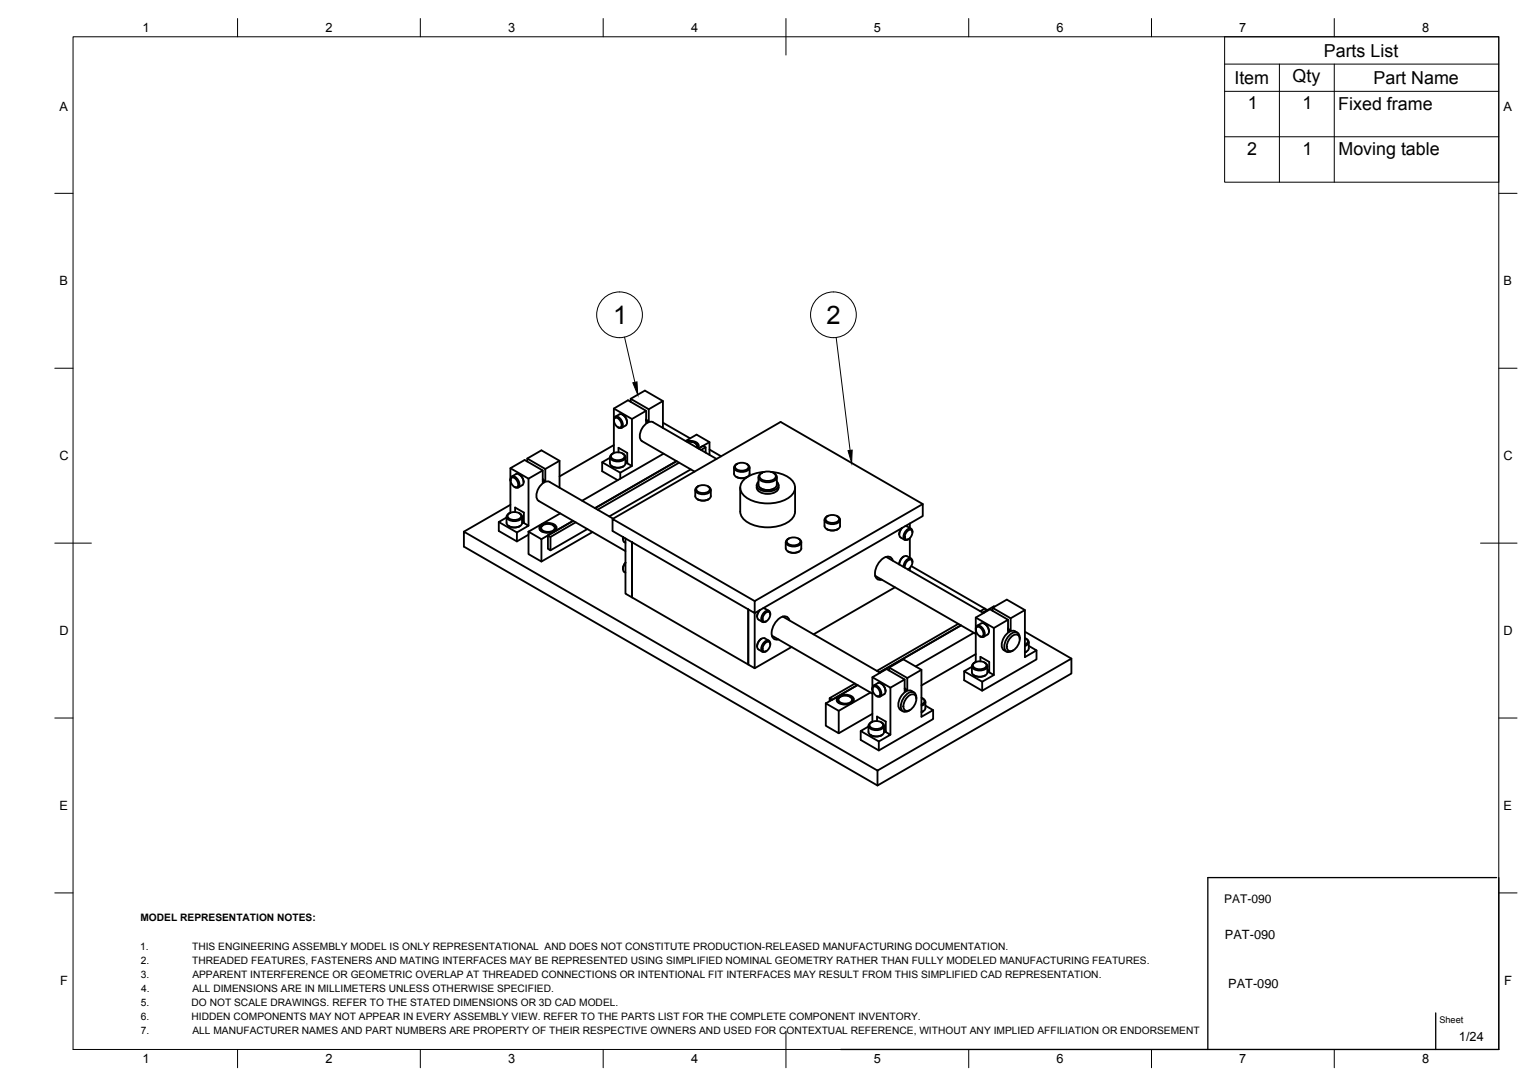
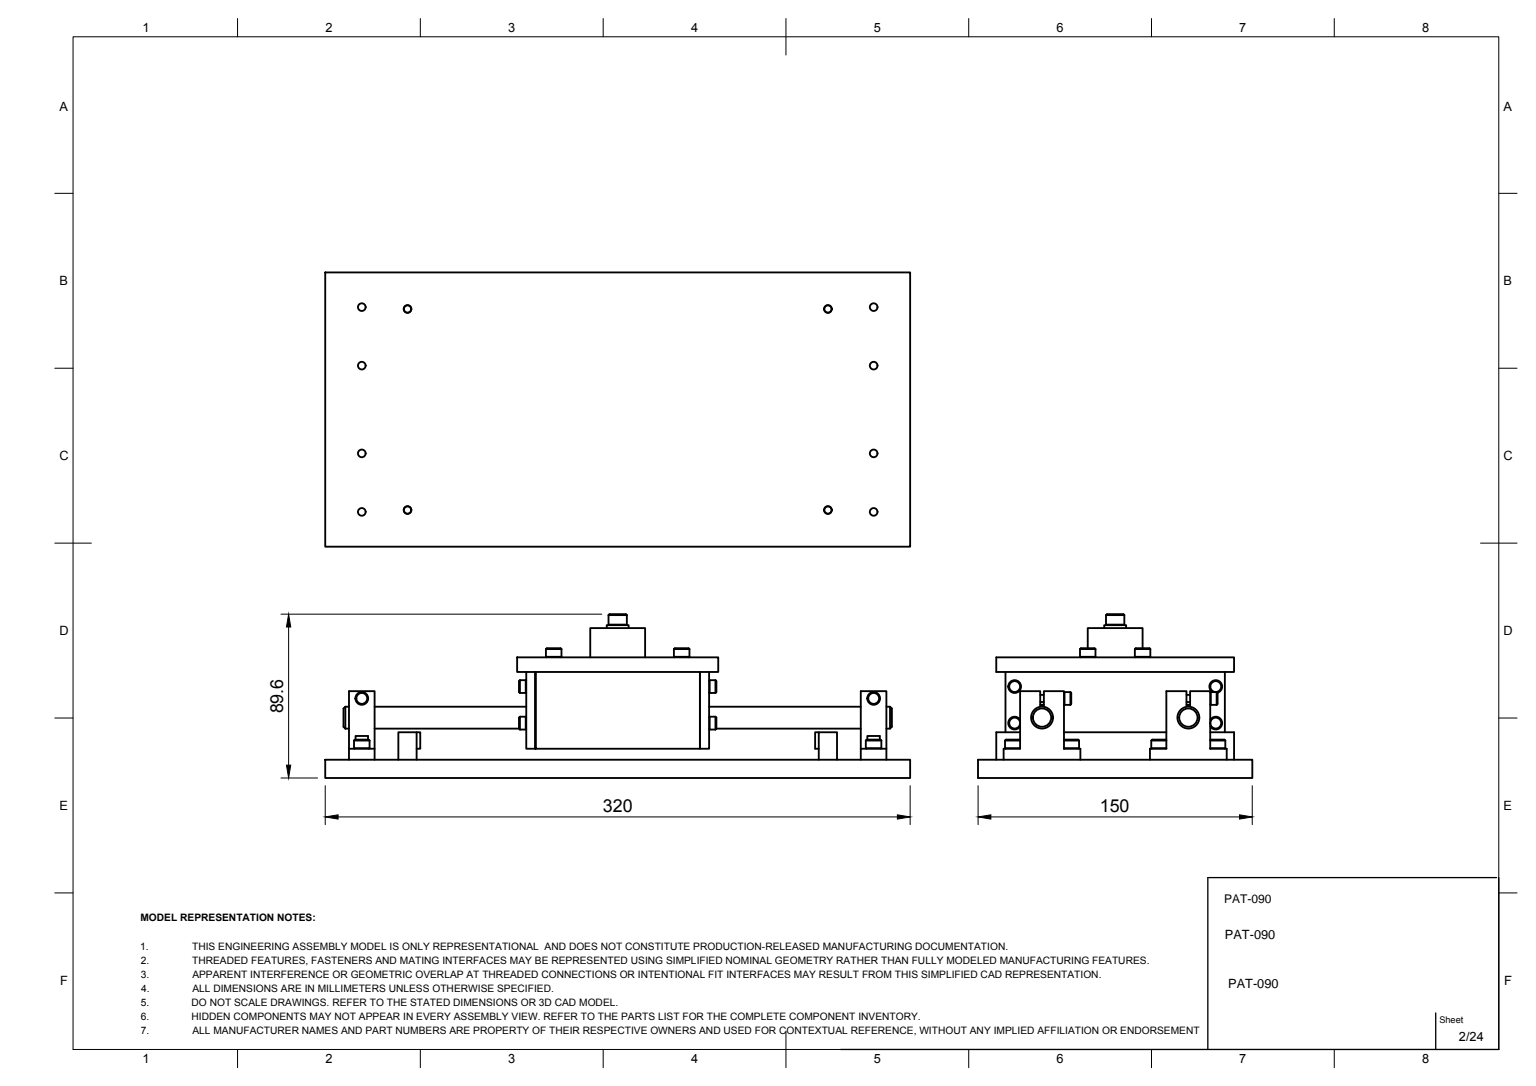
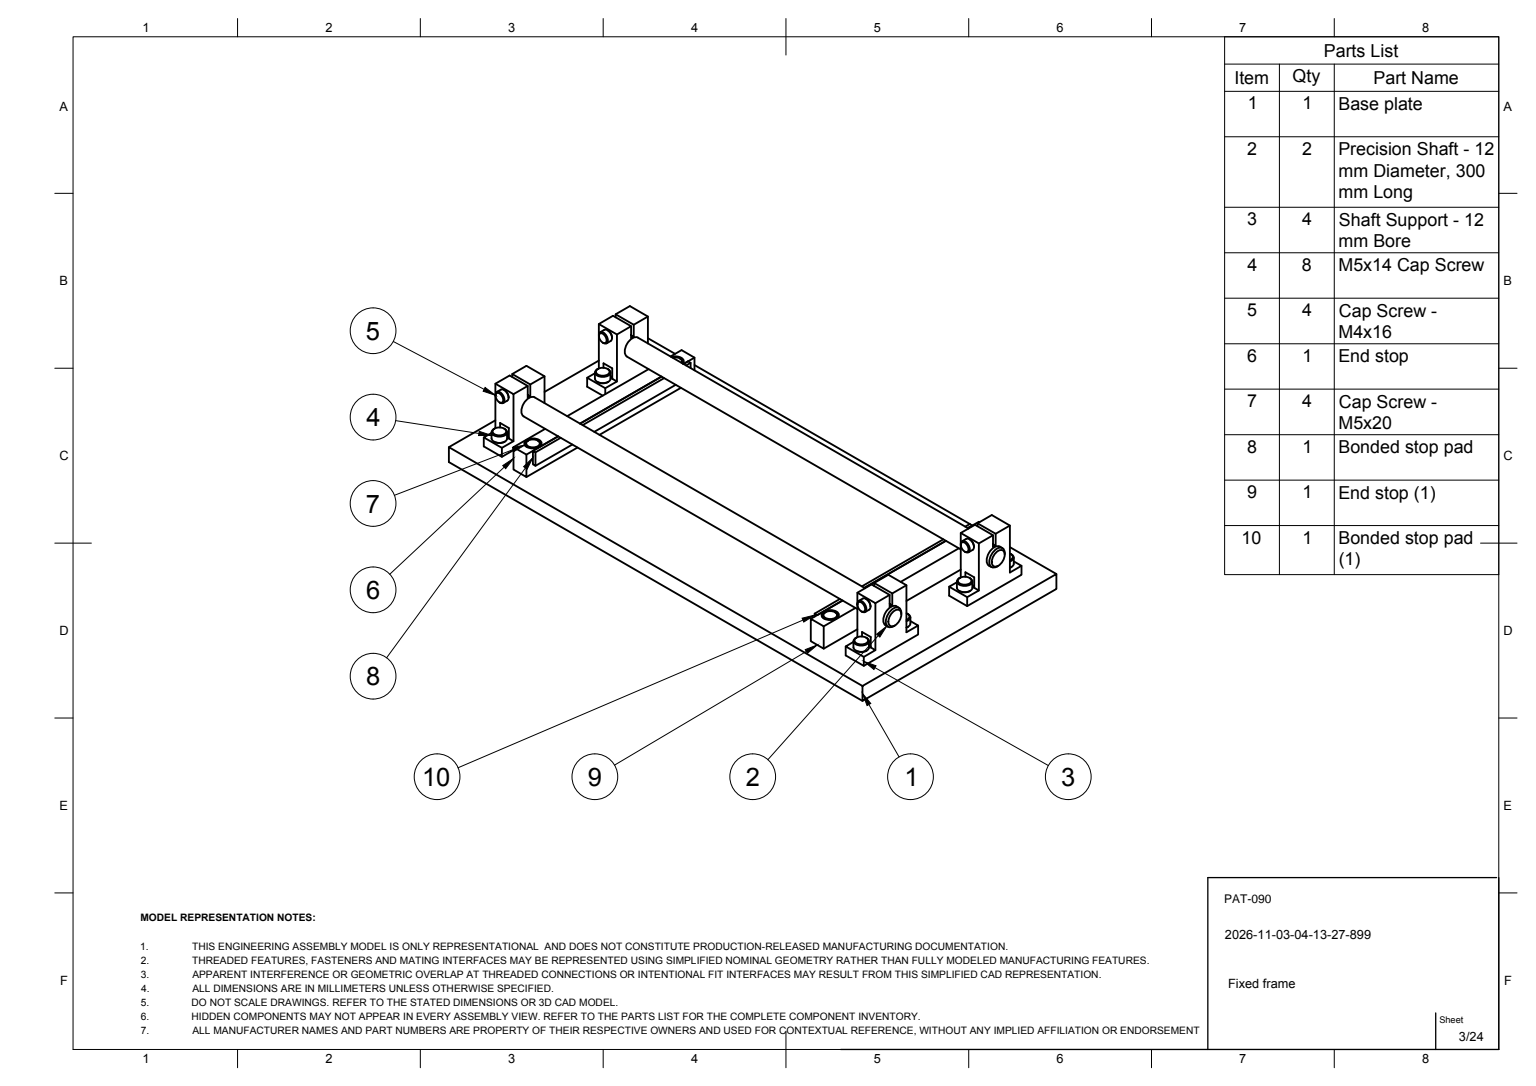
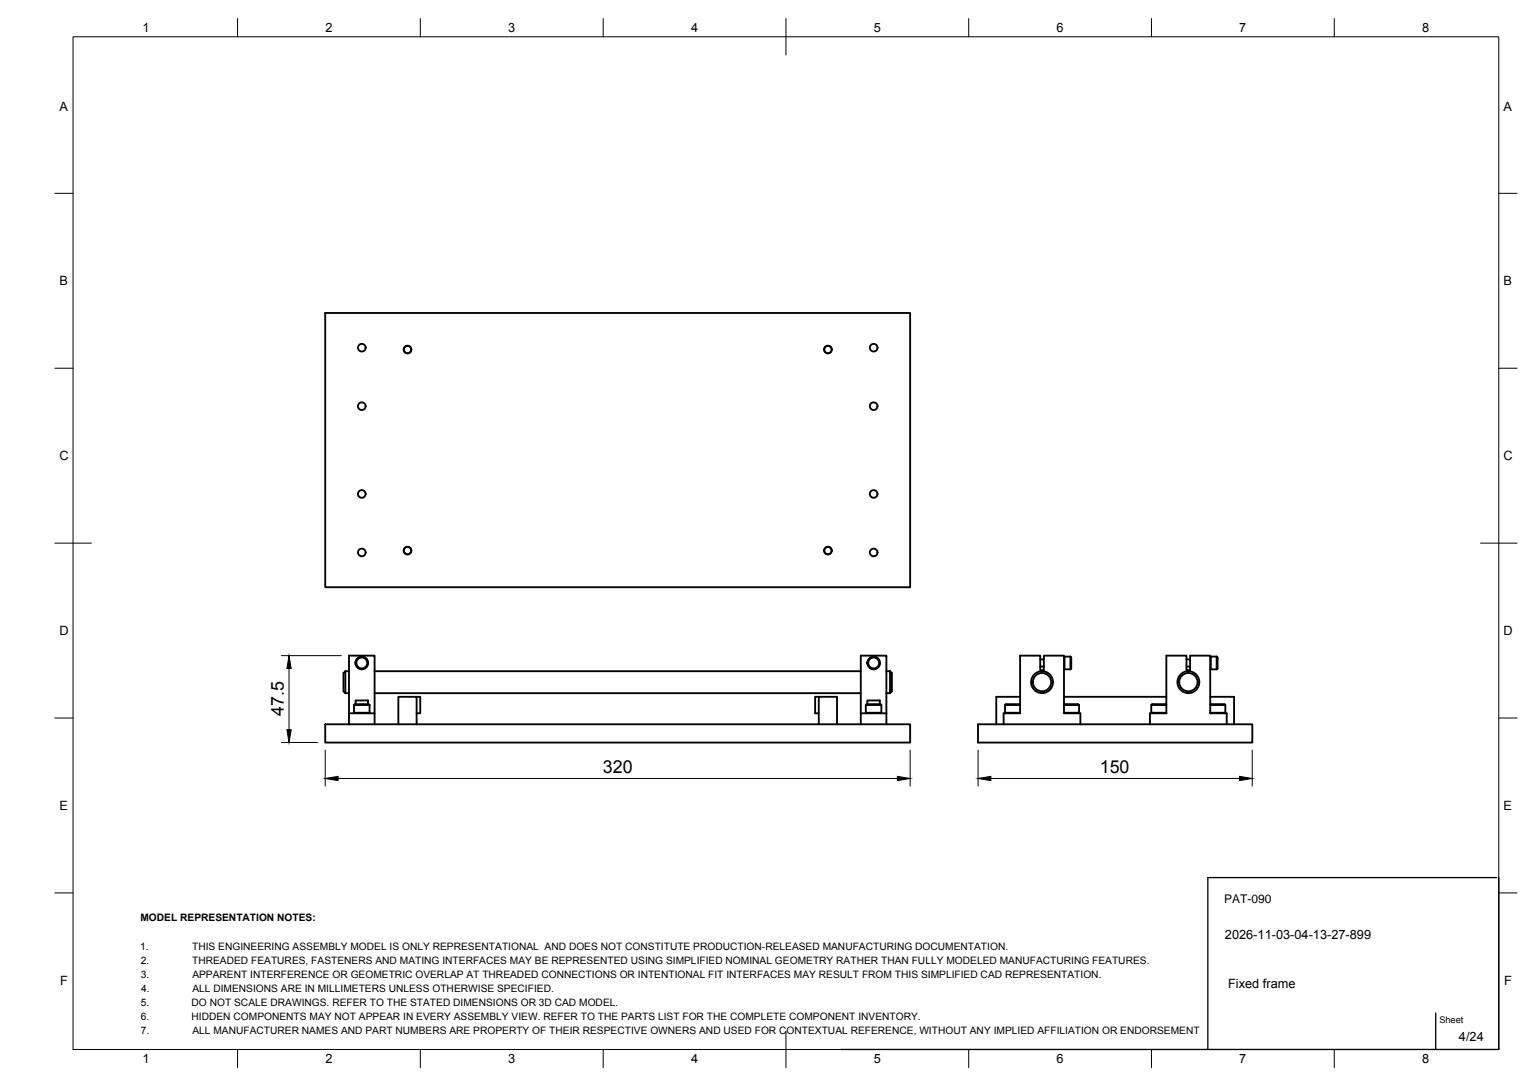
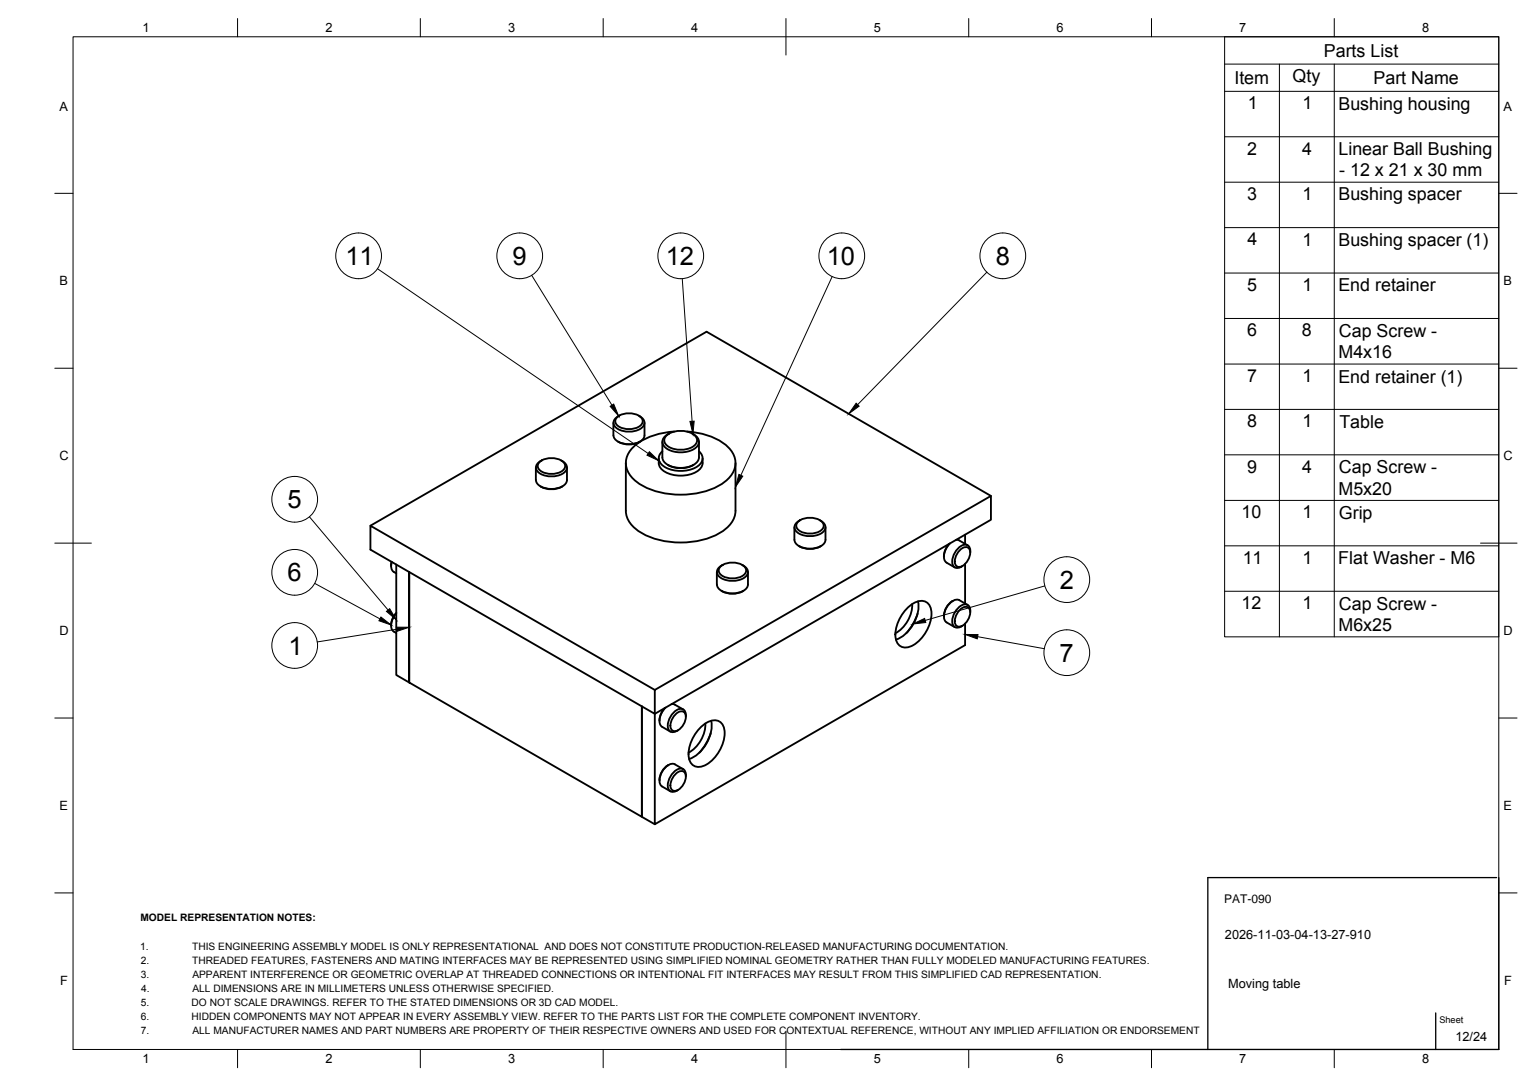
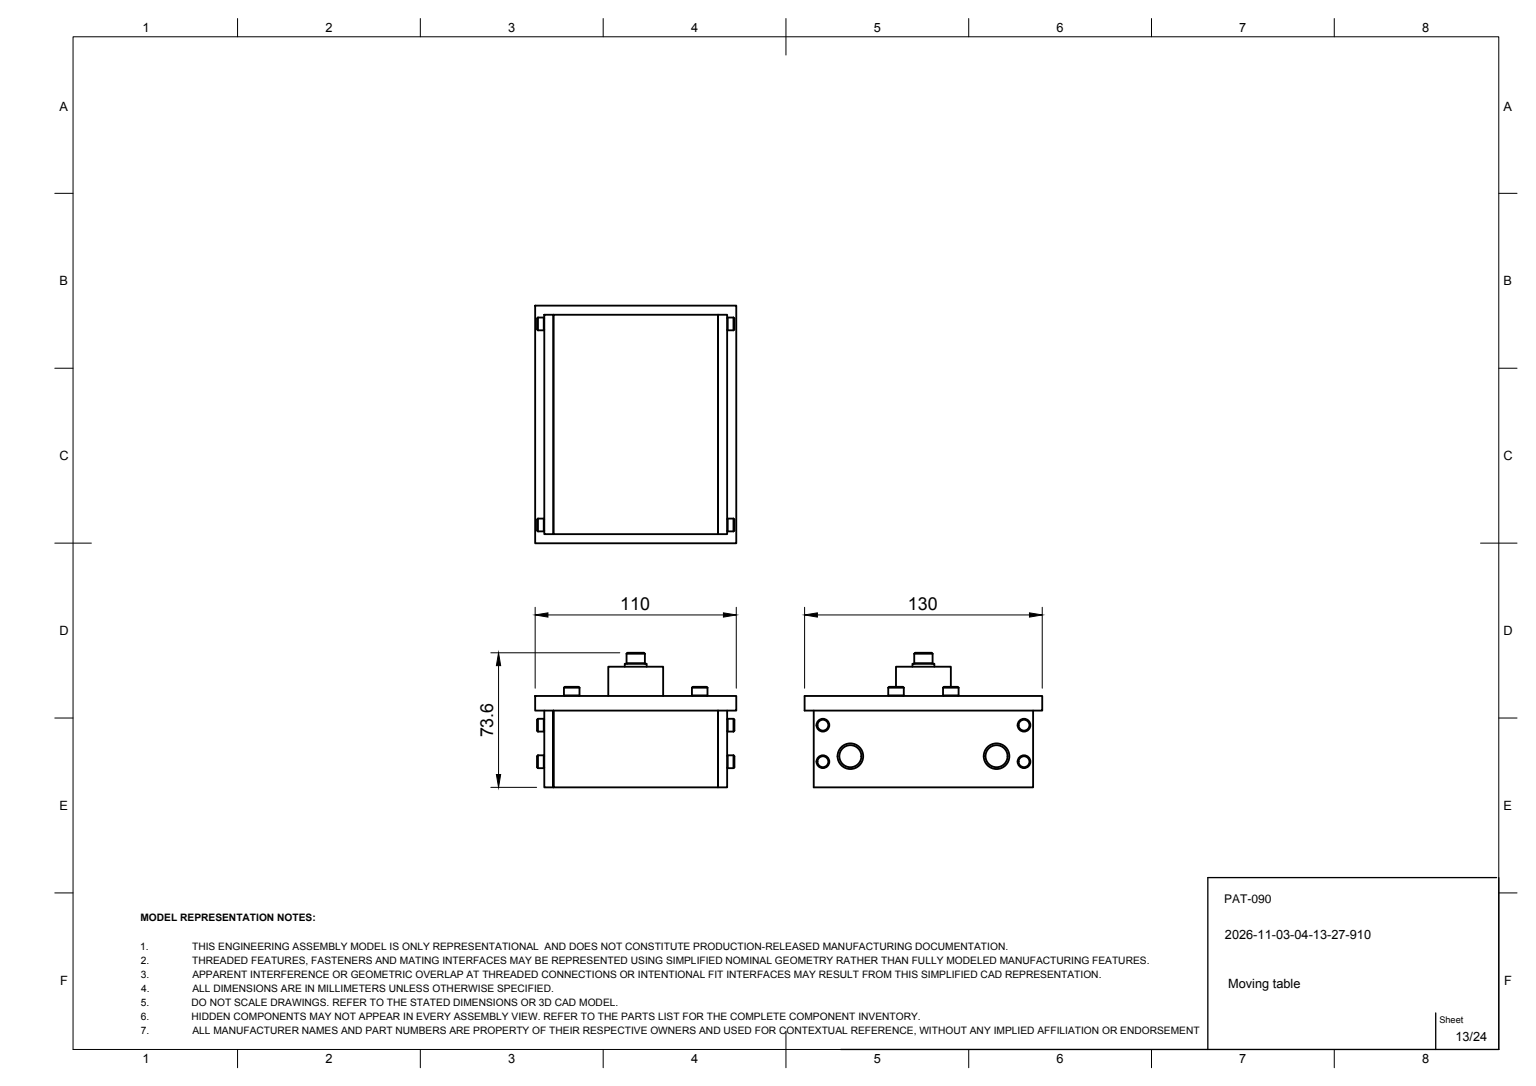
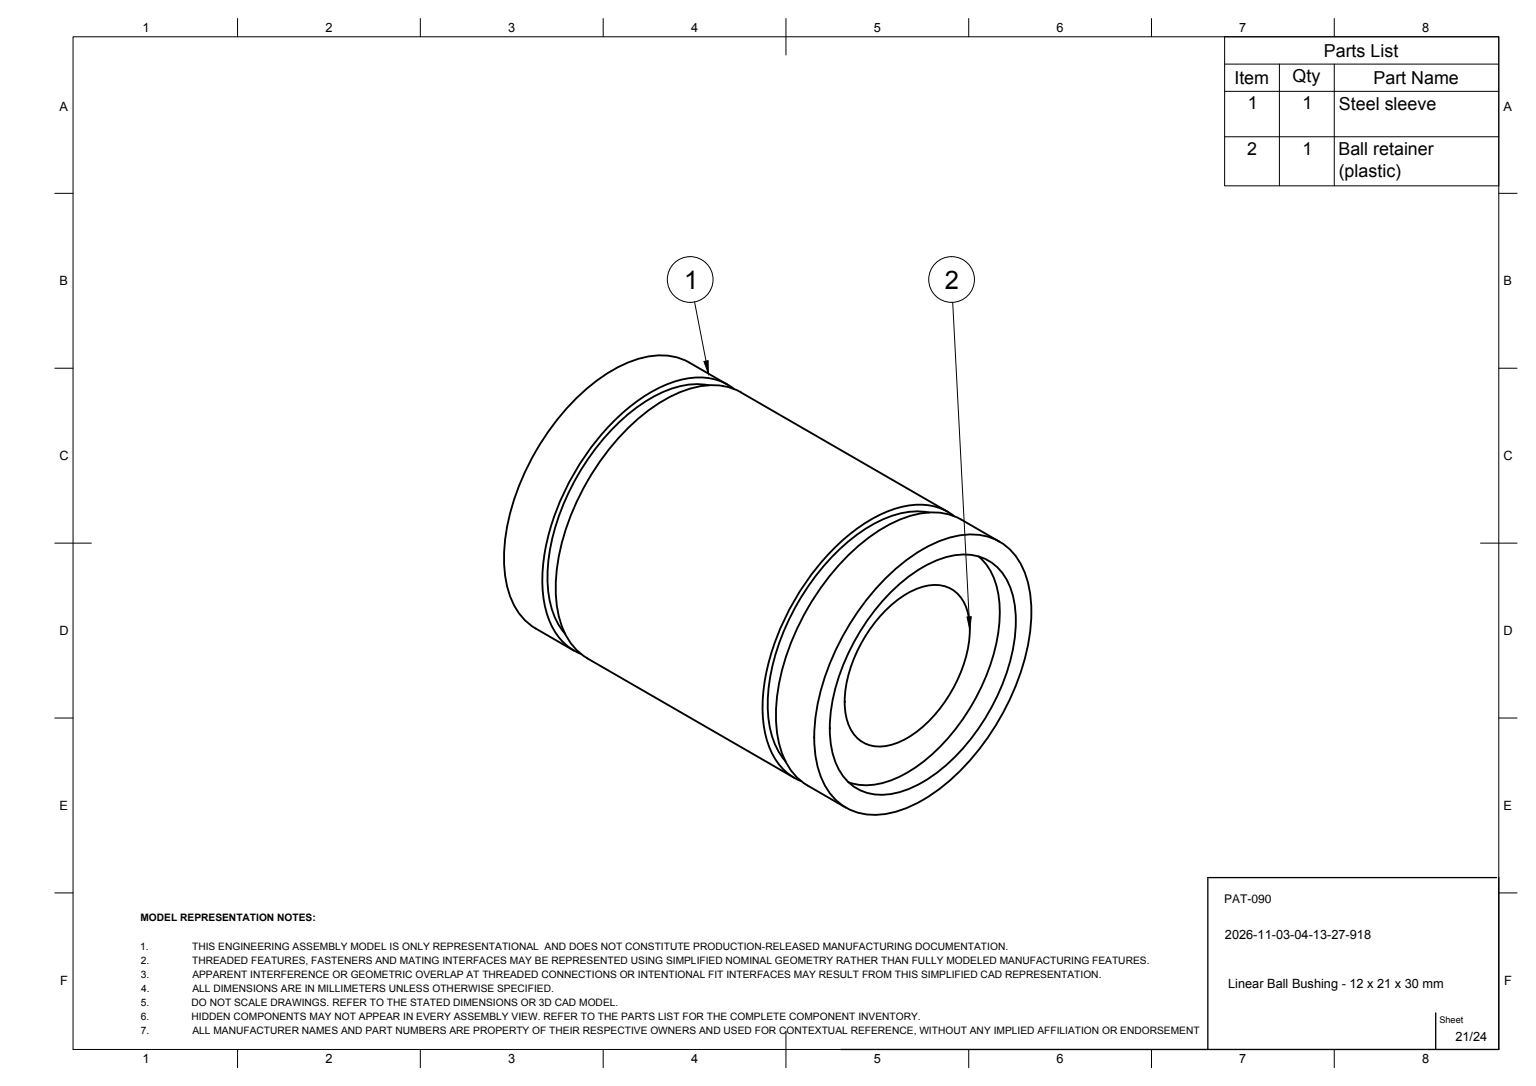
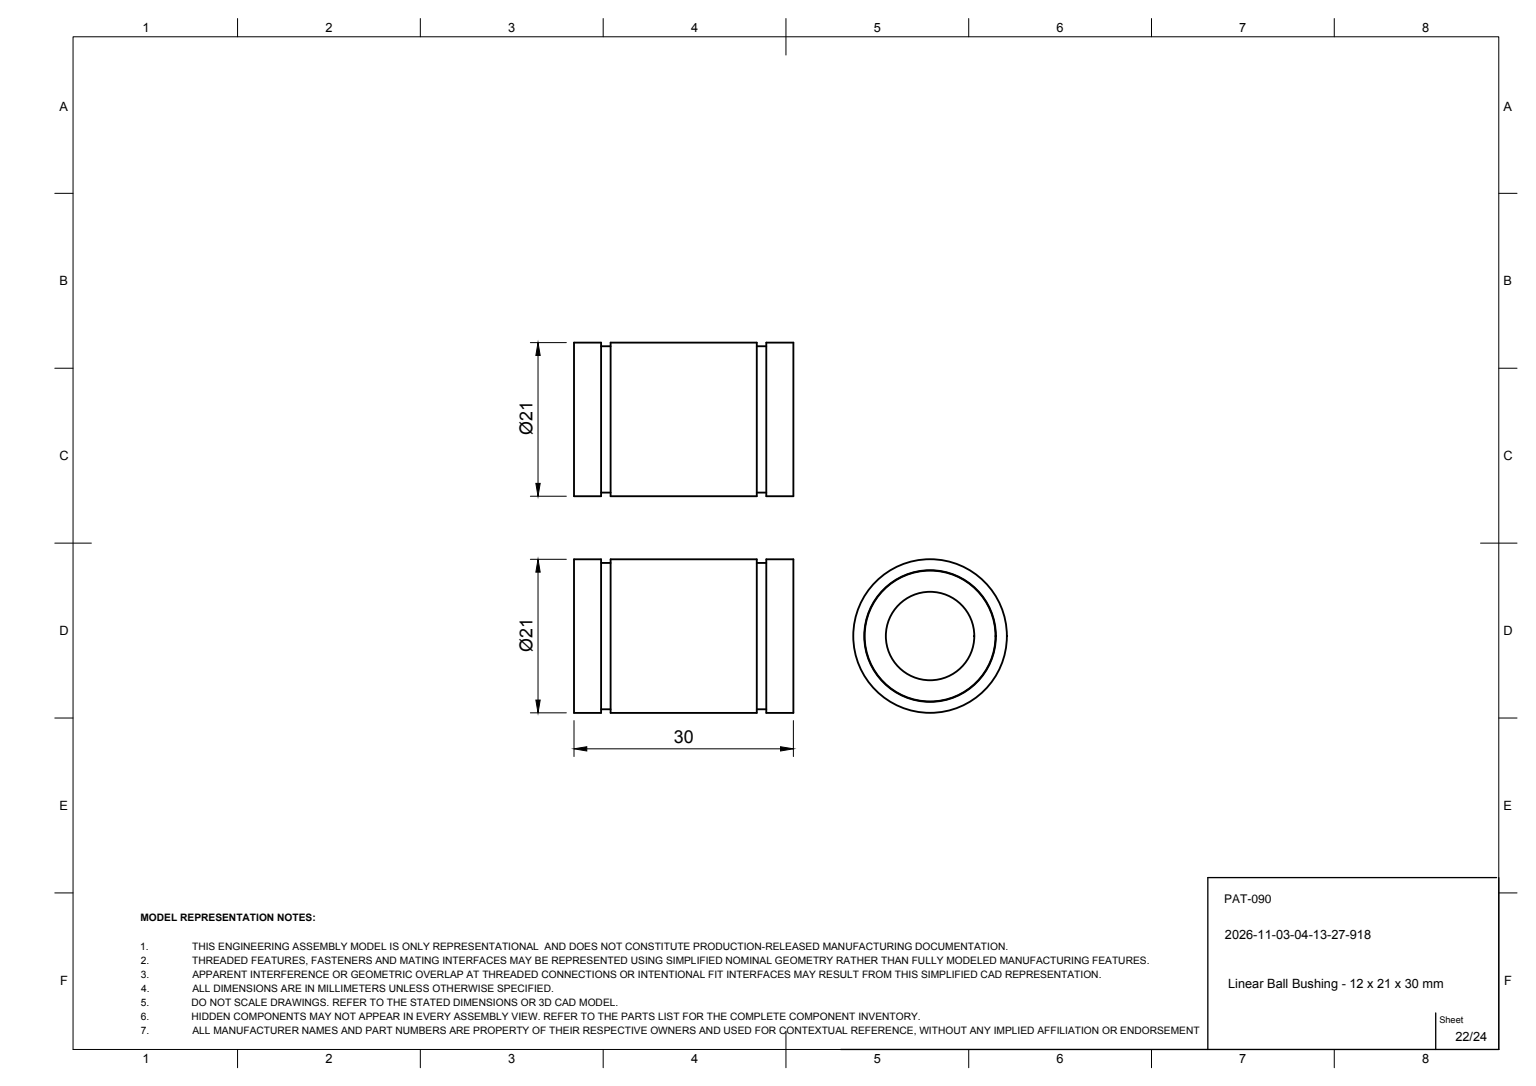
ISO-10303-21;
HEADER;
/* Generated by software containing ST-Developer
 * from STEP Tools, Inc. (www.steptools.com) 
 */

FILE_DESCRIPTION(
/* description */ ('Round-Shaft Linear Stage with Ball Bushings'),
/* implementation_level */ '2;1');

FILE_NAME(
/* name */ 'PAT-090',
/* time_stamp */ '2026-10-27T10:47:55-07:00',
/* author */ (''),
/* organization */ (''),
/* preprocessor_version */ 'ST-DEVELOPER v20.2',
/* originating_system */ 'Autodesk Translation Framework v15.17.0.0',
/* authorisation */ '');

FILE_SCHEMA (('AUTOMOTIVE_DESIGN { 1 0 10303 214 3 1 1 }'));
ENDSEC;

DATA;
#10=MECHANICAL_DESIGN_GEOMETRIC_PRESENTATION_REPRESENTATION('',(#302,#303,
#304,#305,#306,#307,#308,#309,#310,#311,#312,#313,#314,#315,#316,#317,#318,
#319,#320,#321,#322),#7835);
#11=ITEM_DEFINED_TRANSFORMATION($,$,#4984,#5033);
#12=ITEM_DEFINED_TRANSFORMATION($,$,#5016,#5034);
#13=ITEM_DEFINED_TRANSFORMATION($,$,#4651,#5087);
#14=ITEM_DEFINED_TRANSFORMATION($,$,#4694,#5088);
#15=ITEM_DEFINED_TRANSFORMATION($,$,#4715,#5089);
#16=ITEM_DEFINED_TRANSFORMATION($,$,#4722,#5090);
#17=ITEM_DEFINED_TRANSFORMATION($,$,#4743,#5091);
#18=ITEM_DEFINED_TRANSFORMATION($,$,#4750,#5092);
#19=ITEM_DEFINED_TRANSFORMATION($,$,#4760,#5093);
#20=ITEM_DEFINED_TRANSFORMATION($,$,#4798,#5094);
#21=ITEM_DEFINED_TRANSFORMATION($,$,#4798,#5095);
#22=ITEM_DEFINED_TRANSFORMATION($,$,#5035,#5096);
#23=ITEM_DEFINED_TRANSFORMATION($,$,#4760,#5097);
#24=ITEM_DEFINED_TRANSFORMATION($,$,#4798,#5098);
#25=ITEM_DEFINED_TRANSFORMATION($,$,#4798,#5099);
#26=ITEM_DEFINED_TRANSFORMATION($,$,#5035,#5100);
#27=ITEM_DEFINED_TRANSFORMATION($,$,#4750,#5101);
#28=ITEM_DEFINED_TRANSFORMATION($,$,#4760,#5102);
#29=ITEM_DEFINED_TRANSFORMATION($,$,#4798,#5103);
#30=ITEM_DEFINED_TRANSFORMATION($,$,#4798,#5104);
#31=ITEM_DEFINED_TRANSFORMATION($,$,#5035,#5105);
#32=ITEM_DEFINED_TRANSFORMATION($,$,#4760,#5106);
#33=ITEM_DEFINED_TRANSFORMATION($,$,#4798,#5107);
#34=ITEM_DEFINED_TRANSFORMATION($,$,#4798,#5108);
#35=ITEM_DEFINED_TRANSFORMATION($,$,#5035,#5109);
#36=ITEM_DEFINED_TRANSFORMATION($,$,#5061,#5110);
#37=ITEM_DEFINED_TRANSFORMATION($,$,#5061,#5111);
#38=ITEM_DEFINED_TRANSFORMATION($,$,#5061,#5112);
#39=ITEM_DEFINED_TRANSFORMATION($,$,#5061,#5113);
#40=ITEM_DEFINED_TRANSFORMATION($,$,#4823,#5149);
#41=ITEM_DEFINED_TRANSFORMATION($,$,#4884,#5150);
#42=ITEM_DEFINED_TRANSFORMATION($,$,#4893,#5151);
#43=ITEM_DEFINED_TRANSFORMATION($,$,#4902,#5152);
#44=ITEM_DEFINED_TRANSFORMATION($,$,#4927,#5153);
#45=ITEM_DEFINED_TRANSFORMATION($,$,#4952,#5154);
#46=ITEM_DEFINED_TRANSFORMATION($,$,#4974,#5155);
#47=ITEM_DEFINED_TRANSFORMATION($,$,#4983,#5156);
#48=ITEM_DEFINED_TRANSFORMATION($,$,#4983,#5157);
#49=ITEM_DEFINED_TRANSFORMATION($,$,#4983,#5158);
#50=ITEM_DEFINED_TRANSFORMATION($,$,#4983,#5159);
#51=ITEM_DEFINED_TRANSFORMATION($,$,#5035,#5160);
#52=ITEM_DEFINED_TRANSFORMATION($,$,#5035,#5161);
#53=ITEM_DEFINED_TRANSFORMATION($,$,#5035,#5162);
#54=ITEM_DEFINED_TRANSFORMATION($,$,#5035,#5163);
#55=ITEM_DEFINED_TRANSFORMATION($,$,#5035,#5164);
#56=ITEM_DEFINED_TRANSFORMATION($,$,#5035,#5165);
#57=ITEM_DEFINED_TRANSFORMATION($,$,#5035,#5166);
#58=ITEM_DEFINED_TRANSFORMATION($,$,#5035,#5167);
#59=ITEM_DEFINED_TRANSFORMATION($,$,#5061,#5168);
#60=ITEM_DEFINED_TRANSFORMATION($,$,#5061,#5169);
#61=ITEM_DEFINED_TRANSFORMATION($,$,#5061,#5170);
#62=ITEM_DEFINED_TRANSFORMATION($,$,#5061,#5171);
#63=ITEM_DEFINED_TRANSFORMATION($,$,#5114,#5172);
#64=ITEM_DEFINED_TRANSFORMATION($,$,#5123,#5173);
#65=ITEM_DEFINED_TRANSFORMATION($,$,#4650,#5174);
#66=ITEM_DEFINED_TRANSFORMATION($,$,#4822,#5175);
#67=(
REPRESENTATION_RELATIONSHIP($,$,#7965,#7964)
REPRESENTATION_RELATIONSHIP_WITH_TRANSFORMATION(#11)
SHAPE_REPRESENTATION_RELATIONSHIP()
);
#68=(
REPRESENTATION_RELATIONSHIP($,$,#7966,#7964)
REPRESENTATION_RELATIONSHIP_WITH_TRANSFORMATION(#12)
SHAPE_REPRESENTATION_RELATIONSHIP()
);
#69=(
REPRESENTATION_RELATIONSHIP($,$,#7948,#7947)
REPRESENTATION_RELATIONSHIP_WITH_TRANSFORMATION(#13)
SHAPE_REPRESENTATION_RELATIONSHIP()
);
#70=(
REPRESENTATION_RELATIONSHIP($,$,#7949,#7947)
REPRESENTATION_RELATIONSHIP_WITH_TRANSFORMATION(#14)
SHAPE_REPRESENTATION_RELATIONSHIP()
);
#71=(
REPRESENTATION_RELATIONSHIP($,$,#7950,#7947)
REPRESENTATION_RELATIONSHIP_WITH_TRANSFORMATION(#15)
SHAPE_REPRESENTATION_RELATIONSHIP()
);
#72=(
REPRESENTATION_RELATIONSHIP($,$,#7951,#7947)
REPRESENTATION_RELATIONSHIP_WITH_TRANSFORMATION(#16)
SHAPE_REPRESENTATION_RELATIONSHIP()
);
#73=(
REPRESENTATION_RELATIONSHIP($,$,#7952,#7947)
REPRESENTATION_RELATIONSHIP_WITH_TRANSFORMATION(#17)
SHAPE_REPRESENTATION_RELATIONSHIP()
);
#74=(
REPRESENTATION_RELATIONSHIP($,$,#7953,#7947)
REPRESENTATION_RELATIONSHIP_WITH_TRANSFORMATION(#18)
SHAPE_REPRESENTATION_RELATIONSHIP()
);
#75=(
REPRESENTATION_RELATIONSHIP($,$,#7954,#7947)
REPRESENTATION_RELATIONSHIP_WITH_TRANSFORMATION(#19)
SHAPE_REPRESENTATION_RELATIONSHIP()
);
#76=(
REPRESENTATION_RELATIONSHIP($,$,#7955,#7947)
REPRESENTATION_RELATIONSHIP_WITH_TRANSFORMATION(#20)
SHAPE_REPRESENTATION_RELATIONSHIP()
);
#77=(
REPRESENTATION_RELATIONSHIP($,$,#7955,#7947)
REPRESENTATION_RELATIONSHIP_WITH_TRANSFORMATION(#21)
SHAPE_REPRESENTATION_RELATIONSHIP()
);
#78=(
REPRESENTATION_RELATIONSHIP($,$,#7967,#7947)
REPRESENTATION_RELATIONSHIP_WITH_TRANSFORMATION(#22)
SHAPE_REPRESENTATION_RELATIONSHIP()
);
#79=(
REPRESENTATION_RELATIONSHIP($,$,#7954,#7947)
REPRESENTATION_RELATIONSHIP_WITH_TRANSFORMATION(#23)
SHAPE_REPRESENTATION_RELATIONSHIP()
);
#80=(
REPRESENTATION_RELATIONSHIP($,$,#7955,#7947)
REPRESENTATION_RELATIONSHIP_WITH_TRANSFORMATION(#24)
SHAPE_REPRESENTATION_RELATIONSHIP()
);
#81=(
REPRESENTATION_RELATIONSHIP($,$,#7955,#7947)
REPRESENTATION_RELATIONSHIP_WITH_TRANSFORMATION(#25)
SHAPE_REPRESENTATION_RELATIONSHIP()
);
#82=(
REPRESENTATION_RELATIONSHIP($,$,#7967,#7947)
REPRESENTATION_RELATIONSHIP_WITH_TRANSFORMATION(#26)
SHAPE_REPRESENTATION_RELATIONSHIP()
);
#83=(
REPRESENTATION_RELATIONSHIP($,$,#7953,#7947)
REPRESENTATION_RELATIONSHIP_WITH_TRANSFORMATION(#27)
SHAPE_REPRESENTATION_RELATIONSHIP()
);
#84=(
REPRESENTATION_RELATIONSHIP($,$,#7954,#7947)
REPRESENTATION_RELATIONSHIP_WITH_TRANSFORMATION(#28)
SHAPE_REPRESENTATION_RELATIONSHIP()
);
#85=(
REPRESENTATION_RELATIONSHIP($,$,#7955,#7947)
REPRESENTATION_RELATIONSHIP_WITH_TRANSFORMATION(#29)
SHAPE_REPRESENTATION_RELATIONSHIP()
);
#86=(
REPRESENTATION_RELATIONSHIP($,$,#7955,#7947)
REPRESENTATION_RELATIONSHIP_WITH_TRANSFORMATION(#30)
SHAPE_REPRESENTATION_RELATIONSHIP()
);
#87=(
REPRESENTATION_RELATIONSHIP($,$,#7967,#7947)
REPRESENTATION_RELATIONSHIP_WITH_TRANSFORMATION(#31)
SHAPE_REPRESENTATION_RELATIONSHIP()
);
#88=(
REPRESENTATION_RELATIONSHIP($,$,#7954,#7947)
REPRESENTATION_RELATIONSHIP_WITH_TRANSFORMATION(#32)
SHAPE_REPRESENTATION_RELATIONSHIP()
);
#89=(
REPRESENTATION_RELATIONSHIP($,$,#7955,#7947)
REPRESENTATION_RELATIONSHIP_WITH_TRANSFORMATION(#33)
SHAPE_REPRESENTATION_RELATIONSHIP()
);
#90=(
REPRESENTATION_RELATIONSHIP($,$,#7955,#7947)
REPRESENTATION_RELATIONSHIP_WITH_TRANSFORMATION(#34)
SHAPE_REPRESENTATION_RELATIONSHIP()
);
#91=(
REPRESENTATION_RELATIONSHIP($,$,#7967,#7947)
REPRESENTATION_RELATIONSHIP_WITH_TRANSFORMATION(#35)
SHAPE_REPRESENTATION_RELATIONSHIP()
);
#92=(
REPRESENTATION_RELATIONSHIP($,$,#7968,#7947)
REPRESENTATION_RELATIONSHIP_WITH_TRANSFORMATION(#36)
SHAPE_REPRESENTATION_RELATIONSHIP()
);
#93=(
REPRESENTATION_RELATIONSHIP($,$,#7968,#7947)
REPRESENTATION_RELATIONSHIP_WITH_TRANSFORMATION(#37)
SHAPE_REPRESENTATION_RELATIONSHIP()
);
#94=(
REPRESENTATION_RELATIONSHIP($,$,#7968,#7947)
REPRESENTATION_RELATIONSHIP_WITH_TRANSFORMATION(#38)
SHAPE_REPRESENTATION_RELATIONSHIP()
);
#95=(
REPRESENTATION_RELATIONSHIP($,$,#7968,#7947)
REPRESENTATION_RELATIONSHIP_WITH_TRANSFORMATION(#39)
SHAPE_REPRESENTATION_RELATIONSHIP()
);
#96=(
REPRESENTATION_RELATIONSHIP($,$,#7957,#7956)
REPRESENTATION_RELATIONSHIP_WITH_TRANSFORMATION(#40)
SHAPE_REPRESENTATION_RELATIONSHIP()
);
#97=(
REPRESENTATION_RELATIONSHIP($,$,#7958,#7956)
REPRESENTATION_RELATIONSHIP_WITH_TRANSFORMATION(#41)
SHAPE_REPRESENTATION_RELATIONSHIP()
);
#98=(
REPRESENTATION_RELATIONSHIP($,$,#7959,#7956)
REPRESENTATION_RELATIONSHIP_WITH_TRANSFORMATION(#42)
SHAPE_REPRESENTATION_RELATIONSHIP()
);
#99=(
REPRESENTATION_RELATIONSHIP($,$,#7960,#7956)
REPRESENTATION_RELATIONSHIP_WITH_TRANSFORMATION(#43)
SHAPE_REPRESENTATION_RELATIONSHIP()
);
#100=(
REPRESENTATION_RELATIONSHIP($,$,#7961,#7956)
REPRESENTATION_RELATIONSHIP_WITH_TRANSFORMATION(#44)
SHAPE_REPRESENTATION_RELATIONSHIP()
);
#101=(
REPRESENTATION_RELATIONSHIP($,$,#7962,#7956)
REPRESENTATION_RELATIONSHIP_WITH_TRANSFORMATION(#45)
SHAPE_REPRESENTATION_RELATIONSHIP()
);
#102=(
REPRESENTATION_RELATIONSHIP($,$,#7963,#7956)
REPRESENTATION_RELATIONSHIP_WITH_TRANSFORMATION(#46)
SHAPE_REPRESENTATION_RELATIONSHIP()
);
#103=(
REPRESENTATION_RELATIONSHIP($,$,#7964,#7956)
REPRESENTATION_RELATIONSHIP_WITH_TRANSFORMATION(#47)
SHAPE_REPRESENTATION_RELATIONSHIP()
);
#104=(
REPRESENTATION_RELATIONSHIP($,$,#7964,#7956)
REPRESENTATION_RELATIONSHIP_WITH_TRANSFORMATION(#48)
SHAPE_REPRESENTATION_RELATIONSHIP()
);
#105=(
REPRESENTATION_RELATIONSHIP($,$,#7964,#7956)
REPRESENTATION_RELATIONSHIP_WITH_TRANSFORMATION(#49)
SHAPE_REPRESENTATION_RELATIONSHIP()
);
#106=(
REPRESENTATION_RELATIONSHIP($,$,#7964,#7956)
REPRESENTATION_RELATIONSHIP_WITH_TRANSFORMATION(#50)
SHAPE_REPRESENTATION_RELATIONSHIP()
);
#107=(
REPRESENTATION_RELATIONSHIP($,$,#7967,#7956)
REPRESENTATION_RELATIONSHIP_WITH_TRANSFORMATION(#51)
SHAPE_REPRESENTATION_RELATIONSHIP()
);
#108=(
REPRESENTATION_RELATIONSHIP($,$,#7967,#7956)
REPRESENTATION_RELATIONSHIP_WITH_TRANSFORMATION(#52)
SHAPE_REPRESENTATION_RELATIONSHIP()
);
#109=(
REPRESENTATION_RELATIONSHIP($,$,#7967,#7956)
REPRESENTATION_RELATIONSHIP_WITH_TRANSFORMATION(#53)
SHAPE_REPRESENTATION_RELATIONSHIP()
);
#110=(
REPRESENTATION_RELATIONSHIP($,$,#7967,#7956)
REPRESENTATION_RELATIONSHIP_WITH_TRANSFORMATION(#54)
SHAPE_REPRESENTATION_RELATIONSHIP()
);
#111=(
REPRESENTATION_RELATIONSHIP($,$,#7967,#7956)
REPRESENTATION_RELATIONSHIP_WITH_TRANSFORMATION(#55)
SHAPE_REPRESENTATION_RELATIONSHIP()
);
#112=(
REPRESENTATION_RELATIONSHIP($,$,#7967,#7956)
REPRESENTATION_RELATIONSHIP_WITH_TRANSFORMATION(#56)
SHAPE_REPRESENTATION_RELATIONSHIP()
);
#113=(
REPRESENTATION_RELATIONSHIP($,$,#7967,#7956)
REPRESENTATION_RELATIONSHIP_WITH_TRANSFORMATION(#57)
SHAPE_REPRESENTATION_RELATIONSHIP()
);
#114=(
REPRESENTATION_RELATIONSHIP($,$,#7967,#7956)
REPRESENTATION_RELATIONSHIP_WITH_TRANSFORMATION(#58)
SHAPE_REPRESENTATION_RELATIONSHIP()
);
#115=(
REPRESENTATION_RELATIONSHIP($,$,#7968,#7956)
REPRESENTATION_RELATIONSHIP_WITH_TRANSFORMATION(#59)
SHAPE_REPRESENTATION_RELATIONSHIP()
);
#116=(
REPRESENTATION_RELATIONSHIP($,$,#7968,#7956)
REPRESENTATION_RELATIONSHIP_WITH_TRANSFORMATION(#60)
SHAPE_REPRESENTATION_RELATIONSHIP()
);
#117=(
REPRESENTATION_RELATIONSHIP($,$,#7968,#7956)
REPRESENTATION_RELATIONSHIP_WITH_TRANSFORMATION(#61)
SHAPE_REPRESENTATION_RELATIONSHIP()
);
#118=(
REPRESENTATION_RELATIONSHIP($,$,#7968,#7956)
REPRESENTATION_RELATIONSHIP_WITH_TRANSFORMATION(#62)
SHAPE_REPRESENTATION_RELATIONSHIP()
);
#119=(
REPRESENTATION_RELATIONSHIP($,$,#7969,#7956)
REPRESENTATION_RELATIONSHIP_WITH_TRANSFORMATION(#63)
SHAPE_REPRESENTATION_RELATIONSHIP()
);
#120=(
REPRESENTATION_RELATIONSHIP($,$,#7970,#7956)
REPRESENTATION_RELATIONSHIP_WITH_TRANSFORMATION(#64)
SHAPE_REPRESENTATION_RELATIONSHIP()
);
#121=(
REPRESENTATION_RELATIONSHIP($,$,#7947,#7946)
REPRESENTATION_RELATIONSHIP_WITH_TRANSFORMATION(#65)
SHAPE_REPRESENTATION_RELATIONSHIP()
);
#122=(
REPRESENTATION_RELATIONSHIP($,$,#7956,#7946)
REPRESENTATION_RELATIONSHIP_WITH_TRANSFORMATION(#66)
SHAPE_REPRESENTATION_RELATIONSHIP()
);
#123=CONTEXT_DEPENDENT_SHAPE_REPRESENTATION(#67,#7886);
#124=CONTEXT_DEPENDENT_SHAPE_REPRESENTATION(#68,#7887);
#125=CONTEXT_DEPENDENT_SHAPE_REPRESENTATION(#69,#7890);
#126=CONTEXT_DEPENDENT_SHAPE_REPRESENTATION(#70,#7891);
#127=CONTEXT_DEPENDENT_SHAPE_REPRESENTATION(#71,#7892);
#128=CONTEXT_DEPENDENT_SHAPE_REPRESENTATION(#72,#7893);
#129=CONTEXT_DEPENDENT_SHAPE_REPRESENTATION(#73,#7894);
#130=CONTEXT_DEPENDENT_SHAPE_REPRESENTATION(#74,#7895);
#131=CONTEXT_DEPENDENT_SHAPE_REPRESENTATION(#75,#7896);
#132=CONTEXT_DEPENDENT_SHAPE_REPRESENTATION(#76,#7897);
#133=CONTEXT_DEPENDENT_SHAPE_REPRESENTATION(#77,#7898);
#134=CONTEXT_DEPENDENT_SHAPE_REPRESENTATION(#78,#7899);
#135=CONTEXT_DEPENDENT_SHAPE_REPRESENTATION(#79,#7900);
#136=CONTEXT_DEPENDENT_SHAPE_REPRESENTATION(#80,#7901);
#137=CONTEXT_DEPENDENT_SHAPE_REPRESENTATION(#81,#7902);
#138=CONTEXT_DEPENDENT_SHAPE_REPRESENTATION(#82,#7903);
#139=CONTEXT_DEPENDENT_SHAPE_REPRESENTATION(#83,#7904);
#140=CONTEXT_DEPENDENT_SHAPE_REPRESENTATION(#84,#7905);
#141=CONTEXT_DEPENDENT_SHAPE_REPRESENTATION(#85,#7906);
#142=CONTEXT_DEPENDENT_SHAPE_REPRESENTATION(#86,#7907);
#143=CONTEXT_DEPENDENT_SHAPE_REPRESENTATION(#87,#7908);
#144=CONTEXT_DEPENDENT_SHAPE_REPRESENTATION(#88,#7909);
#145=CONTEXT_DEPENDENT_SHAPE_REPRESENTATION(#89,#7910);
#146=CONTEXT_DEPENDENT_SHAPE_REPRESENTATION(#90,#7911);
#147=CONTEXT_DEPENDENT_SHAPE_REPRESENTATION(#91,#7912);
#148=CONTEXT_DEPENDENT_SHAPE_REPRESENTATION(#92,#7913);
#149=CONTEXT_DEPENDENT_SHAPE_REPRESENTATION(#93,#7914);
#150=CONTEXT_DEPENDENT_SHAPE_REPRESENTATION(#94,#7915);
#151=CONTEXT_DEPENDENT_SHAPE_REPRESENTATION(#95,#7916);
#152=CONTEXT_DEPENDENT_SHAPE_REPRESENTATION(#96,#7919);
#153=CONTEXT_DEPENDENT_SHAPE_REPRESENTATION(#97,#7920);
#154=CONTEXT_DEPENDENT_SHAPE_REPRESENTATION(#98,#7921);
#155=CONTEXT_DEPENDENT_SHAPE_REPRESENTATION(#99,#7922);
#156=CONTEXT_DEPENDENT_SHAPE_REPRESENTATION(#100,#7923);
#157=CONTEXT_DEPENDENT_SHAPE_REPRESENTATION(#101,#7924);
#158=CONTEXT_DEPENDENT_SHAPE_REPRESENTATION(#102,#7925);
#159=CONTEXT_DEPENDENT_SHAPE_REPRESENTATION(#103,#7926);
#160=CONTEXT_DEPENDENT_SHAPE_REPRESENTATION(#104,#7927);
#161=CONTEXT_DEPENDENT_SHAPE_REPRESENTATION(#105,#7928);
#162=CONTEXT_DEPENDENT_SHAPE_REPRESENTATION(#106,#7929);
#163=CONTEXT_DEPENDENT_SHAPE_REPRESENTATION(#107,#7930);
#164=CONTEXT_DEPENDENT_SHAPE_REPRESENTATION(#108,#7931);
#165=CONTEXT_DEPENDENT_SHAPE_REPRESENTATION(#109,#7932);
#166=CONTEXT_DEPENDENT_SHAPE_REPRESENTATION(#110,#7933);
#167=CONTEXT_DEPENDENT_SHAPE_REPRESENTATION(#111,#7934);
#168=CONTEXT_DEPENDENT_SHAPE_REPRESENTATION(#112,#7935);
#169=CONTEXT_DEPENDENT_SHAPE_REPRESENTATION(#113,#7936);
#170=CONTEXT_DEPENDENT_SHAPE_REPRESENTATION(#114,#7937);
#171=CONTEXT_DEPENDENT_SHAPE_REPRESENTATION(#115,#7938);
#172=CONTEXT_DEPENDENT_SHAPE_REPRESENTATION(#116,#7939);
#173=CONTEXT_DEPENDENT_SHAPE_REPRESENTATION(#117,#7940);
#174=CONTEXT_DEPENDENT_SHAPE_REPRESENTATION(#118,#7941);
#175=CONTEXT_DEPENDENT_SHAPE_REPRESENTATION(#119,#7942);
#176=CONTEXT_DEPENDENT_SHAPE_REPRESENTATION(#120,#7943);
#177=CONTEXT_DEPENDENT_SHAPE_REPRESENTATION(#121,#7944);
#178=CONTEXT_DEPENDENT_SHAPE_REPRESENTATION(#122,#7945);
#179=NEXT_ASSEMBLY_USAGE_OCCURRENCE('Steel sleeve:1','Steel sleeve:1',
'Steel sleeve:1',#7990,#7991,'Steel sleeve:1');
#180=NEXT_ASSEMBLY_USAGE_OCCURRENCE('Ball retainer (plastic):1',
'Ball retainer (plastic):1','Ball retainer (plastic):1',#7990,#7992,
'Ball retainer (plastic):1');
#181=NEXT_ASSEMBLY_USAGE_OCCURRENCE('Base plate:1','Base plate:1',
'Base plate:1',#7973,#7974,'Base plate:1');
#182=NEXT_ASSEMBLY_USAGE_OCCURRENCE('End stop:1','End stop:1',
'End stop:1',#7973,#7975,'End stop:1');
#183=NEXT_ASSEMBLY_USAGE_OCCURRENCE('Bonded stop pad:1',
'Bonded stop pad:1','Bonded stop pad:1',#7973,#7976,'Bonded stop pad:1');
#184=NEXT_ASSEMBLY_USAGE_OCCURRENCE('End stop (1):1','End stop (1):1',
'End stop (1):1',#7973,#7977,'End stop (1):1');
#185=NEXT_ASSEMBLY_USAGE_OCCURRENCE('Bonded stop pad (1):1',
'Bonded stop pad (1):1','Bonded stop pad (1):1',#7973,#7978,
'Bonded stop pad (1):1');
#186=NEXT_ASSEMBLY_USAGE_OCCURRENCE(
'Precision Shaft - 12 mm Diameter, 300 mm Long:2',
'Precision Shaft - 12 mm Diameter, 300 mm Long:2',
'Precision Shaft - 12 mm Diameter, 300 mm Long:2',#7973,#7979,
'Precision Shaft - 12 mm Diameter, 300 mm Long:2');
#187=NEXT_ASSEMBLY_USAGE_OCCURRENCE('Shaft Support - 12 mm Bore:2',
'Shaft Support - 12 mm Bore:2','Shaft Support - 12 mm Bore:2',#7973,#7980,
'Shaft Support - 12 mm Bore:2');
#188=NEXT_ASSEMBLY_USAGE_OCCURRENCE('M5x14 Cap Screw:2',
'M5x14 Cap Screw:2','M5x14 Cap Screw:2',#7973,#7981,'M5x14 Cap Screw:2');
#189=NEXT_ASSEMBLY_USAGE_OCCURRENCE('M5x14 Cap Screw:3',
'M5x14 Cap Screw:3','M5x14 Cap Screw:3',#7973,#7981,'M5x14 Cap Screw:3');
#190=NEXT_ASSEMBLY_USAGE_OCCURRENCE('Cap Screw - M4x16:2',
'Cap Screw - M4x16:2','Cap Screw - M4x16:2',#7973,#7993,
'Cap Screw - M4x16:2');
#191=NEXT_ASSEMBLY_USAGE_OCCURRENCE('Shaft Support - 12 mm Bore:3',
'Shaft Support - 12 mm Bore:3','Shaft Support - 12 mm Bore:3',#7973,#7980,
'Shaft Support - 12 mm Bore:3');
#192=NEXT_ASSEMBLY_USAGE_OCCURRENCE('M5x14 Cap Screw:4',
'M5x14 Cap Screw:4','M5x14 Cap Screw:4',#7973,#7981,'M5x14 Cap Screw:4');
#193=NEXT_ASSEMBLY_USAGE_OCCURRENCE('M5x14 Cap Screw:5',
'M5x14 Cap Screw:5','M5x14 Cap Screw:5',#7973,#7981,'M5x14 Cap Screw:5');
#194=NEXT_ASSEMBLY_USAGE_OCCURRENCE('Cap Screw - M4x16:3',
'Cap Screw - M4x16:3','Cap Screw - M4x16:3',#7973,#7993,
'Cap Screw - M4x16:3');
#195=NEXT_ASSEMBLY_USAGE_OCCURRENCE(
'Precision Shaft - 12 mm Diameter, 300 mm Long:3',
'Precision Shaft - 12 mm Diameter, 300 mm Long:3',
'Precision Shaft - 12 mm Diameter, 300 mm Long:3',#7973,#7979,
'Precision Shaft - 12 mm Diameter, 300 mm Long:3');
#196=NEXT_ASSEMBLY_USAGE_OCCURRENCE('Shaft Support - 12 mm Bore:4',
'Shaft Support - 12 mm Bore:4','Shaft Support - 12 mm Bore:4',#7973,#7980,
'Shaft Support - 12 mm Bore:4');
#197=NEXT_ASSEMBLY_USAGE_OCCURRENCE('M5x14 Cap Screw:6',
'M5x14 Cap Screw:6','M5x14 Cap Screw:6',#7973,#7981,'M5x14 Cap Screw:6');
#198=NEXT_ASSEMBLY_USAGE_OCCURRENCE('M5x14 Cap Screw:7',
'M5x14 Cap Screw:7','M5x14 Cap Screw:7',#7973,#7981,'M5x14 Cap Screw:7');
#199=NEXT_ASSEMBLY_USAGE_OCCURRENCE('Cap Screw - M4x16:4',
'Cap Screw - M4x16:4','Cap Screw - M4x16:4',#7973,#7993,
'Cap Screw - M4x16:4');
#200=NEXT_ASSEMBLY_USAGE_OCCURRENCE('Shaft Support - 12 mm Bore:5',
'Shaft Support - 12 mm Bore:5','Shaft Support - 12 mm Bore:5',#7973,#7980,
'Shaft Support - 12 mm Bore:5');
#201=NEXT_ASSEMBLY_USAGE_OCCURRENCE('M5x14 Cap Screw:8',
'M5x14 Cap Screw:8','M5x14 Cap Screw:8',#7973,#7981,'M5x14 Cap Screw:8');
#202=NEXT_ASSEMBLY_USAGE_OCCURRENCE('M5x14 Cap Screw:9',
'M5x14 Cap Screw:9','M5x14 Cap Screw:9',#7973,#7981,'M5x14 Cap Screw:9');
#203=NEXT_ASSEMBLY_USAGE_OCCURRENCE('Cap Screw - M4x16:5',
'Cap Screw - M4x16:5','Cap Screw - M4x16:5',#7973,#7993,
'Cap Screw - M4x16:5');
#204=NEXT_ASSEMBLY_USAGE_OCCURRENCE('Cap Screw - M5x20:6',
'Cap Screw - M5x20:6','Cap Screw - M5x20:6',#7973,#7994,
'Cap Screw - M5x20:6');
#205=NEXT_ASSEMBLY_USAGE_OCCURRENCE('Cap Screw - M5x20:7',
'Cap Screw - M5x20:7','Cap Screw - M5x20:7',#7973,#7994,
'Cap Screw - M5x20:7');
#206=NEXT_ASSEMBLY_USAGE_OCCURRENCE('Cap Screw - M5x20:8',
'Cap Screw - M5x20:8','Cap Screw - M5x20:8',#7973,#7994,
'Cap Screw - M5x20:8');
#207=NEXT_ASSEMBLY_USAGE_OCCURRENCE('Cap Screw - M5x20:9',
'Cap Screw - M5x20:9','Cap Screw - M5x20:9',#7973,#7994,
'Cap Screw - M5x20:9');
#208=NEXT_ASSEMBLY_USAGE_OCCURRENCE('Bushing housing:1',
'Bushing housing:1','Bushing housing:1',#7982,#7983,'Bushing housing:1');
#209=NEXT_ASSEMBLY_USAGE_OCCURRENCE('Bushing spacer:1',
'Bushing spacer:1','Bushing spacer:1',#7982,#7984,'Bushing spacer:1');
#210=NEXT_ASSEMBLY_USAGE_OCCURRENCE('Bushing spacer (1):1',
'Bushing spacer (1):1','Bushing spacer (1):1',#7982,#7985,
'Bushing spacer (1):1');
#211=NEXT_ASSEMBLY_USAGE_OCCURRENCE('End retainer:1','End retainer:1',
'End retainer:1',#7982,#7986,'End retainer:1');
#212=NEXT_ASSEMBLY_USAGE_OCCURRENCE('End retainer (1):1',
'End retainer (1):1','End retainer (1):1',#7982,#7987,
'End retainer (1):1');
#213=NEXT_ASSEMBLY_USAGE_OCCURRENCE('Table:1','Table:1','Table:1',#7982,
#7988,'Table:1');
#214=NEXT_ASSEMBLY_USAGE_OCCURRENCE('Grip:1','Grip:1','Grip:1',#7982,#7989,
'Grip:1');
#215=NEXT_ASSEMBLY_USAGE_OCCURRENCE(
'Linear Ball Bushing - 12 x 21 x 30 mm:2',
'Linear Ball Bushing - 12 x 21 x 30 mm:2',
'Linear Ball Bushing - 12 x 21 x 30 mm:2',#7982,#7990,
'Linear Ball Bushing - 12 x 21 x 30 mm:2');
#216=NEXT_ASSEMBLY_USAGE_OCCURRENCE(
'Linear Ball Bushing - 12 x 21 x 30 mm:3',
'Linear Ball Bushing - 12 x 21 x 30 mm:3',
'Linear Ball Bushing - 12 x 21 x 30 mm:3',#7982,#7990,
'Linear Ball Bushing - 12 x 21 x 30 mm:3');
#217=NEXT_ASSEMBLY_USAGE_OCCURRENCE(
'Linear Ball Bushing - 12 x 21 x 30 mm:4',
'Linear Ball Bushing - 12 x 21 x 30 mm:4',
'Linear Ball Bushing - 12 x 21 x 30 mm:4',#7982,#7990,
'Linear Ball Bushing - 12 x 21 x 30 mm:4');
#218=NEXT_ASSEMBLY_USAGE_OCCURRENCE(
'Linear Ball Bushing - 12 x 21 x 30 mm:5',
'Linear Ball Bushing - 12 x 21 x 30 mm:5',
'Linear Ball Bushing - 12 x 21 x 30 mm:5',#7982,#7990,
'Linear Ball Bushing - 12 x 21 x 30 mm:5');
#219=NEXT_ASSEMBLY_USAGE_OCCURRENCE('Cap Screw - M4x16:6',
'Cap Screw - M4x16:6','Cap Screw - M4x16:6',#7982,#7993,
'Cap Screw - M4x16:6');
#220=NEXT_ASSEMBLY_USAGE_OCCURRENCE('Cap Screw - M4x16:7',
'Cap Screw - M4x16:7','Cap Screw - M4x16:7',#7982,#7993,
'Cap Screw - M4x16:7');
#221=NEXT_ASSEMBLY_USAGE_OCCURRENCE('Cap Screw - M4x16:8',
'Cap Screw - M4x16:8','Cap Screw - M4x16:8',#7982,#7993,
'Cap Screw - M4x16:8');
#222=NEXT_ASSEMBLY_USAGE_OCCURRENCE('Cap Screw - M4x16:9',
'Cap Screw - M4x16:9','Cap Screw - M4x16:9',#7982,#7993,
'Cap Screw - M4x16:9');
#223=NEXT_ASSEMBLY_USAGE_OCCURRENCE('Cap Screw - M4x16:10',
'Cap Screw - M4x16:10','Cap Screw - M4x16:10',#7982,#7993,
'Cap Screw - M4x16:10');
#224=NEXT_ASSEMBLY_USAGE_OCCURRENCE('Cap Screw - M4x16:11',
'Cap Screw - M4x16:11','Cap Screw - M4x16:11',#7982,#7993,
'Cap Screw - M4x16:11');
#225=NEXT_ASSEMBLY_USAGE_OCCURRENCE('Cap Screw - M4x16:12',
'Cap Screw - M4x16:12','Cap Screw - M4x16:12',#7982,#7993,
'Cap Screw - M4x16:12');
#226=NEXT_ASSEMBLY_USAGE_OCCURRENCE('Cap Screw - M4x16:13',
'Cap Screw - M4x16:13','Cap Screw - M4x16:13',#7982,#7993,
'Cap Screw - M4x16:13');
#227=NEXT_ASSEMBLY_USAGE_OCCURRENCE('Cap Screw - M5x20:2',
'Cap Screw - M5x20:2','Cap Screw - M5x20:2',#7982,#7994,
'Cap Screw - M5x20:2');
#228=NEXT_ASSEMBLY_USAGE_OCCURRENCE('Cap Screw - M5x20:3',
'Cap Screw - M5x20:3','Cap Screw - M5x20:3',#7982,#7994,
'Cap Screw - M5x20:3');
#229=NEXT_ASSEMBLY_USAGE_OCCURRENCE('Cap Screw - M5x20:4',
'Cap Screw - M5x20:4','Cap Screw - M5x20:4',#7982,#7994,
'Cap Screw - M5x20:4');
#230=NEXT_ASSEMBLY_USAGE_OCCURRENCE('Cap Screw - M5x20:5',
'Cap Screw - M5x20:5','Cap Screw - M5x20:5',#7982,#7994,
'Cap Screw - M5x20:5');
#231=NEXT_ASSEMBLY_USAGE_OCCURRENCE('Flat Washer - M6:2',
'Flat Washer - M6:2','Flat Washer - M6:2',#7982,#7995,
'Flat Washer - M6:2');
#232=NEXT_ASSEMBLY_USAGE_OCCURRENCE('Cap Screw - M6x25:2',
'Cap Screw - M6x25:2','Cap Screw - M6x25:2',#7982,#7996,
'Cap Screw - M6x25:2');
#233=NEXT_ASSEMBLY_USAGE_OCCURRENCE('Fixed frame:1','Fixed frame:1',
'Fixed frame:1',#7972,#7973,'Fixed frame:1');
#234=NEXT_ASSEMBLY_USAGE_OCCURRENCE('Moving table:1','Moving table:1',
'Moving table:1',#7972,#7982,'Moving table:1');
#235=ORIENTED_CLOSED_SHELL('',*,#4399,.F.);
#236=ORIENTED_CLOSED_SHELL('',*,#4411,.F.);
#237=ORIENTED_CLOSED_SHELL('',*,#4413,.F.);
#238=ORIENTED_CLOSED_SHELL('',*,#4416,.F.);
#239=BREP_WITH_VOIDS('Body1',#4400,(#235));
#240=BREP_WITH_VOIDS('Body1',#4410,(#236));
#241=BREP_WITH_VOIDS('Body1',#4412,(#237));
#242=BREP_WITH_VOIDS('Body1',#4415,(#238));
#243=CONICAL_SURFACE('',#4751,0.55,0.785398163397448);
#244=CONICAL_SURFACE('',#4757,0.55,0.785398163397441);
#245=CONICAL_SURFACE('',#4811,0.4,0.785398163397448);
#246=CONICAL_SURFACE('',#4815,0.41,0.785398163397448);
#247=CONICAL_SURFACE('',#4819,0.26,0.463647609000806);
#248=CONICAL_SURFACE('',#5038,0.325,0.785398163397448);
#249=CONICAL_SURFACE('',#5042,0.335,0.785398163397448);
#250=CONICAL_SURFACE('',#5046,0.21,0.463647609000806);
#251=CONICAL_SURFACE('',#5050,0.18,0.785398163397448);
#252=CONICAL_SURFACE('',#5064,0.4,0.785398163397448);
#253=CONICAL_SURFACE('',#5068,0.41,0.785398163397448);
#254=CONICAL_SURFACE('',#5072,0.26,0.463647609000806);
#255=CONICAL_SURFACE('',#5076,0.225,0.785398163397448);
#256=CONICAL_SURFACE('',#5126,0.475,0.785398163397449);
#257=CONICAL_SURFACE('',#5130,0.485,0.785398163397448);
#258=CONICAL_SURFACE('',#5134,0.31,0.463647609000806);
#259=CONICAL_SURFACE('',#5138,0.27,0.785398163397448);
#260=SHAPE_REPRESENTATION_RELATIONSHIP('SRR','None',#7948,#281);
#261=SHAPE_REPRESENTATION_RELATIONSHIP('SRR','None',#7949,#282);
#262=SHAPE_REPRESENTATION_RELATIONSHIP('SRR','None',#7950,#283);
#263=SHAPE_REPRESENTATION_RELATIONSHIP('SRR','None',#7951,#284);
#264=SHAPE_REPRESENTATION_RELATIONSHIP('SRR','None',#7952,#285);
#265=SHAPE_REPRESENTATION_RELATIONSHIP('SRR','None',#7953,#286);
#266=SHAPE_REPRESENTATION_RELATIONSHIP('SRR','None',#7954,#287);
#267=SHAPE_REPRESENTATION_RELATIONSHIP('SRR','None',#7955,#288);
#268=SHAPE_REPRESENTATION_RELATIONSHIP('SRR','None',#7957,#289);
#269=SHAPE_REPRESENTATION_RELATIONSHIP('SRR','None',#7958,#290);
#270=SHAPE_REPRESENTATION_RELATIONSHIP('SRR','None',#7959,#291);
#271=SHAPE_REPRESENTATION_RELATIONSHIP('SRR','None',#7960,#292);
#272=SHAPE_REPRESENTATION_RELATIONSHIP('SRR','None',#7961,#293);
#273=SHAPE_REPRESENTATION_RELATIONSHIP('SRR','None',#7962,#294);
#274=SHAPE_REPRESENTATION_RELATIONSHIP('SRR','None',#7963,#295);
#275=SHAPE_REPRESENTATION_RELATIONSHIP('SRR','None',#7965,#296);
#276=SHAPE_REPRESENTATION_RELATIONSHIP('SRR','None',#7966,#297);
#277=SHAPE_REPRESENTATION_RELATIONSHIP('SRR','None',#7967,#298);
#278=SHAPE_REPRESENTATION_RELATIONSHIP('SRR','None',#7968,#299);
#279=SHAPE_REPRESENTATION_RELATIONSHIP('SRR','None',#7969,#300);
#280=SHAPE_REPRESENTATION_RELATIONSHIP('SRR','None',#7970,#301);
#281=ADVANCED_BREP_SHAPE_REPRESENTATION('',(#323),#7812);
#282=ADVANCED_BREP_SHAPE_REPRESENTATION('',(#324),#7813);
#283=ADVANCED_BREP_SHAPE_REPRESENTATION('',(#325),#7814);
#284=ADVANCED_BREP_SHAPE_REPRESENTATION('',(#326),#7815);
#285=ADVANCED_BREP_SHAPE_REPRESENTATION('',(#327),#7816);
#286=ADVANCED_BREP_SHAPE_REPRESENTATION('',(#328),#7817);
#287=ADVANCED_BREP_SHAPE_REPRESENTATION('',(#329),#7818);
#288=ADVANCED_BREP_SHAPE_REPRESENTATION('',(#239),#7819);
#289=ADVANCED_BREP_SHAPE_REPRESENTATION('',(#330),#7821);
#290=ADVANCED_BREP_SHAPE_REPRESENTATION('',(#331),#7822);
#291=ADVANCED_BREP_SHAPE_REPRESENTATION('',(#332),#7823);
#292=ADVANCED_BREP_SHAPE_REPRESENTATION('',(#333),#7824);
#293=ADVANCED_BREP_SHAPE_REPRESENTATION('',(#334),#7825);
#294=ADVANCED_BREP_SHAPE_REPRESENTATION('',(#335),#7826);
#295=ADVANCED_BREP_SHAPE_REPRESENTATION('',(#336),#7827);
#296=ADVANCED_BREP_SHAPE_REPRESENTATION('',(#337),#7829);
#297=ADVANCED_BREP_SHAPE_REPRESENTATION('',(#338),#7830);
#298=ADVANCED_BREP_SHAPE_REPRESENTATION('',(#240),#7831);
#299=ADVANCED_BREP_SHAPE_REPRESENTATION('',(#241),#7832);
#300=ADVANCED_BREP_SHAPE_REPRESENTATION('',(#339),#7833);
#301=ADVANCED_BREP_SHAPE_REPRESENTATION('',(#242),#7834);
#302=STYLED_ITEM('',(#8123),#323);
#303=STYLED_ITEM('',(#8137),#324);
#304=STYLED_ITEM('',(#8158),#325);
#305=STYLED_ITEM('',(#8137),#326);
#306=STYLED_ITEM('',(#8158),#327);
#307=STYLED_ITEM('',(#8144),#328);
#308=STYLED_ITEM('',(#8144),#329);
#309=STYLED_ITEM('',(#8151),#239);
#310=STYLED_ITEM('',(#8123),#330);
#311=STYLED_ITEM('',(#8158),#331);
#312=STYLED_ITEM('',(#8158),#332);
#313=STYLED_ITEM('',(#8130),#333);
#314=STYLED_ITEM('',(#8130),#334);
#315=STYLED_ITEM('',(#8158),#335);
#316=STYLED_ITEM('',(#8151),#336);
#317=STYLED_ITEM('',(#8158),#337);
#318=STYLED_ITEM('',(#8137),#338);
#319=STYLED_ITEM('',(#8151),#240);
#320=STYLED_ITEM('',(#8151),#241);
#321=STYLED_ITEM('',(#8151),#339);
#322=STYLED_ITEM('',(#8151),#242);
#323=MANIFOLD_SOLID_BREP('Body1',#4392);
#324=MANIFOLD_SOLID_BREP('Body1',#4393);
#325=MANIFOLD_SOLID_BREP('Body1',#4394);
#326=MANIFOLD_SOLID_BREP('Body1',#4395);
#327=MANIFOLD_SOLID_BREP('Body1',#4396);
#328=MANIFOLD_SOLID_BREP('Body1',#4397);
#329=MANIFOLD_SOLID_BREP('Body1',#4398);
#330=MANIFOLD_SOLID_BREP('Body1',#4401);
#331=MANIFOLD_SOLID_BREP('Body1',#4402);
#332=MANIFOLD_SOLID_BREP('Body1',#4403);
#333=MANIFOLD_SOLID_BREP('Body1',#4404);
#334=MANIFOLD_SOLID_BREP('Body1',#4405);
#335=MANIFOLD_SOLID_BREP('Body1',#4406);
#336=MANIFOLD_SOLID_BREP('Body1',#4407);
#337=MANIFOLD_SOLID_BREP('Body1',#4408);
#338=MANIFOLD_SOLID_BREP('Body1',#4409);
#339=MANIFOLD_SOLID_BREP('Body1',#4414);
#340=FACE_BOUND('',#890,.T.);
#341=FACE_BOUND('',#891,.T.);
#342=FACE_BOUND('',#892,.T.);
#343=FACE_BOUND('',#893,.T.);
#344=FACE_BOUND('',#894,.T.);
#345=FACE_BOUND('',#895,.T.);
#346=FACE_BOUND('',#896,.T.);
#347=FACE_BOUND('',#897,.T.);
#348=FACE_BOUND('',#898,.T.);
#349=FACE_BOUND('',#899,.T.);
#350=FACE_BOUND('',#900,.T.);
#351=FACE_BOUND('',#901,.T.);
#352=FACE_BOUND('',#903,.T.);
#353=FACE_BOUND('',#904,.T.);
#354=FACE_BOUND('',#905,.T.);
#355=FACE_BOUND('',#906,.T.);
#356=FACE_BOUND('',#907,.T.);
#357=FACE_BOUND('',#908,.T.);
#358=FACE_BOUND('',#909,.T.);
#359=FACE_BOUND('',#910,.T.);
#360=FACE_BOUND('',#911,.T.);
#361=FACE_BOUND('',#912,.T.);
#362=FACE_BOUND('',#913,.T.);
#363=FACE_BOUND('',#914,.T.);
#364=FACE_BOUND('',#917,.T.);
#365=FACE_BOUND('',#920,.T.);
#366=FACE_BOUND('',#928,.T.);
#367=FACE_BOUND('',#929,.T.);
#368=FACE_BOUND('',#931,.T.);
#369=FACE_BOUND('',#932,.T.);
#370=FACE_BOUND('',#941,.T.);
#371=FACE_BOUND('',#944,.T.);
#372=FACE_BOUND('',#952,.T.);
#373=FACE_BOUND('',#953,.T.);
#374=FACE_BOUND('',#955,.T.);
#375=FACE_BOUND('',#956,.T.);
#376=FACE_BOUND('',#973,.T.);
#377=FACE_BOUND('',#975,.T.);
#378=FACE_BOUND('',#977,.T.);
#379=FACE_BOUND('',#984,.T.);
#380=FACE_BOUND('',#987,.T.);
#381=FACE_BOUND('',#988,.T.);
#382=FACE_BOUND('',#991,.T.);
#383=FACE_BOUND('',#994,.T.);
#384=FACE_BOUND('',#997,.T.);
#385=FACE_BOUND('',#1000,.T.);
#386=FACE_BOUND('',#1015,.T.);
#387=FACE_BOUND('',#1046,.T.);
#388=FACE_BOUND('',#1047,.T.);
#389=FACE_BOUND('',#1048,.T.);
#390=FACE_BOUND('',#1049,.T.);
#391=FACE_BOUND('',#1050,.T.);
#392=FACE_BOUND('',#1051,.T.);
#393=FACE_BOUND('',#1054,.T.);
#394=FACE_BOUND('',#1055,.T.);
#395=FACE_BOUND('',#1056,.T.);
#396=FACE_BOUND('',#1057,.T.);
#397=FACE_BOUND('',#1058,.T.);
#398=FACE_BOUND('',#1059,.T.);
#399=FACE_BOUND('',#1061,.T.);
#400=FACE_BOUND('',#1062,.T.);
#401=FACE_BOUND('',#1063,.T.);
#402=FACE_BOUND('',#1064,.T.);
#403=FACE_BOUND('',#1069,.T.);
#404=FACE_BOUND('',#1071,.T.);
#405=FACE_BOUND('',#1075,.T.);
#406=FACE_BOUND('',#1077,.T.);
#407=FACE_BOUND('',#1086,.T.);
#408=FACE_BOUND('',#1087,.T.);
#409=FACE_BOUND('',#1088,.T.);
#410=FACE_BOUND('',#1089,.T.);
#411=FACE_BOUND('',#1090,.T.);
#412=FACE_BOUND('',#1091,.T.);
#413=FACE_BOUND('',#1094,.T.);
#414=FACE_BOUND('',#1095,.T.);
#415=FACE_BOUND('',#1096,.T.);
#416=FACE_BOUND('',#1097,.T.);
#417=FACE_BOUND('',#1098,.T.);
#418=FACE_BOUND('',#1099,.T.);
#419=FACE_BOUND('',#1110,.T.);
#420=FACE_BOUND('',#1111,.T.);
#421=FACE_BOUND('',#1112,.T.);
#422=FACE_BOUND('',#1113,.T.);
#423=FACE_BOUND('',#1114,.T.);
#424=FACE_BOUND('',#1115,.T.);
#425=FACE_BOUND('',#1118,.T.);
#426=FACE_BOUND('',#1119,.T.);
#427=FACE_BOUND('',#1120,.T.);
#428=FACE_BOUND('',#1121,.T.);
#429=FACE_BOUND('',#1122,.T.);
#430=FACE_BOUND('',#1123,.T.);
#431=FACE_BOUND('',#1136,.T.);
#432=FACE_BOUND('',#1137,.T.);
#433=FACE_BOUND('',#1138,.T.);
#434=FACE_BOUND('',#1139,.T.);
#435=FACE_BOUND('',#1140,.T.);
#436=FACE_BOUND('',#1142,.T.);
#437=FACE_BOUND('',#1143,.T.);
#438=FACE_BOUND('',#1144,.T.);
#439=FACE_BOUND('',#1145,.T.);
#440=FACE_BOUND('',#1146,.T.);
#441=FACE_BOUND('',#1150,.T.);
#442=FACE_BOUND('',#1152,.T.);
#443=FACE_BOUND('',#1159,.T.);
#444=FACE_BOUND('',#1162,.T.);
#445=FACE_BOUND('',#1165,.T.);
#446=FACE_BOUND('',#1168,.T.);
#447=FACE_BOUND('',#1171,.T.);
#448=FACE_BOUND('',#1174,.T.);
#449=FACE_BOUND('',#1176,.T.);
#450=FACE_BOUND('',#1182,.T.);
#451=FACE_BOUND('',#1184,.T.);
#452=FACE_BOUND('',#1186,.T.);
#453=FACE_BOUND('',#1188,.T.);
#454=FACE_BOUND('',#1194,.T.);
#455=FACE_BOUND('',#1212,.T.);
#456=FACE_BOUND('',#1228,.T.);
#457=FACE_BOUND('',#1230,.T.);
#458=FACE_BOUND('',#1236,.T.);
#459=PLANE('',#4688);
#460=PLANE('',#4689);
#461=PLANE('',#4690);
#462=PLANE('',#4691);
#463=PLANE('',#4692);
#464=PLANE('',#4693);
#465=PLANE('',#4698);
#466=PLANE('',#4703);
#467=PLANE('',#4709);
#468=PLANE('',#4710);
#469=PLANE('',#4711);
#470=PLANE('',#4712);
#471=PLANE('',#4713);
#472=PLANE('',#4714);
#473=PLANE('',#4716);
#474=PLANE('',#4717);
#475=PLANE('',#4718);
#476=PLANE('',#4719);
#477=PLANE('',#4720);
#478=PLANE('',#4721);
#479=PLANE('',#4726);
#480=PLANE('',#4731);
#481=PLANE('',#4737);
#482=PLANE('',#4738);
#483=PLANE('',#4739);
#484=PLANE('',#4740);
#485=PLANE('',#4741);
#486=PLANE('',#4742);
#487=PLANE('',#4744);
#488=PLANE('',#4745);
#489=PLANE('',#4746);
#490=PLANE('',#4747);
#491=PLANE('',#4748);
#492=PLANE('',#4749);
#493=PLANE('',#4756);
#494=PLANE('',#4759);
#495=PLANE('',#4761);
#496=PLANE('',#4768);
#497=PLANE('',#4769);
#498=PLANE('',#4771);
#499=PLANE('',#4773);
#500=PLANE('',#4787);
#501=PLANE('',#4788);
#502=PLANE('',#4789);
#503=PLANE('',#4790);
#504=PLANE('',#4791);
#505=PLANE('',#4792);
#506=PLANE('',#4793);
#507=PLANE('',#4794);
#508=PLANE('',#4795);
#509=PLANE('',#4796);
#510=PLANE('',#4797);
#511=PLANE('',#4799);
#512=PLANE('',#4800);
#513=PLANE('',#4801);
#514=PLANE('',#4802);
#515=PLANE('',#4803);
#516=PLANE('',#4804);
#517=PLANE('',#4805);
#518=PLANE('',#4806);
#519=PLANE('',#4807);
#520=PLANE('',#4809);
#521=PLANE('',#4817);
#522=PLANE('',#4827);
#523=PLANE('',#4831);
#524=PLANE('',#4835);
#525=PLANE('',#4839);
#526=PLANE('',#4843);
#527=PLANE('',#4847);
#528=PLANE('',#4851);
#529=PLANE('',#4855);
#530=PLANE('',#4859);
#531=PLANE('',#4863);
#532=PLANE('',#4867);
#533=PLANE('',#4871);
#534=PLANE('',#4878);
#535=PLANE('',#4879);
#536=PLANE('',#4880);
#537=PLANE('',#4881);
#538=PLANE('',#4882);
#539=PLANE('',#4883);
#540=PLANE('',#4891);
#541=PLANE('',#4892);
#542=PLANE('',#4900);
#543=PLANE('',#4901);
#544=PLANE('',#4921);
#545=PLANE('',#4922);
#546=PLANE('',#4923);
#547=PLANE('',#4924);
#548=PLANE('',#4925);
#549=PLANE('',#4926);
#550=PLANE('',#4946);
#551=PLANE('',#4947);
#552=PLANE('',#4948);
#553=PLANE('',#4949);
#554=PLANE('',#4950);
#555=PLANE('',#4951);
#556=PLANE('',#4968);
#557=PLANE('',#4969);
#558=PLANE('',#4970);
#559=PLANE('',#4971);
#560=PLANE('',#4972);
#561=PLANE('',#4973);
#562=PLANE('',#4981);
#563=PLANE('',#4982);
#564=PLANE('',#4985);
#565=PLANE('',#4987);
#566=PLANE('',#4988);
#567=PLANE('',#4990);
#568=PLANE('',#4991);
#569=PLANE('',#4992);
#570=PLANE('',#4997);
#571=PLANE('',#5001);
#572=PLANE('',#5005);
#573=PLANE('',#5009);
#574=PLANE('',#5013);
#575=PLANE('',#5017);
#576=PLANE('',#5020);
#577=PLANE('',#5021);
#578=PLANE('',#5024);
#579=PLANE('',#5025);
#580=PLANE('',#5030);
#581=PLANE('',#5036);
#582=PLANE('',#5044);
#583=PLANE('',#5052);
#584=PLANE('',#5053);
#585=PLANE('',#5054);
#586=PLANE('',#5055);
#587=PLANE('',#5056);
#588=PLANE('',#5057);
#589=PLANE('',#5058);
#590=PLANE('',#5059);
#591=PLANE('',#5060);
#592=PLANE('',#5062);
#593=PLANE('',#5070);
#594=PLANE('',#5078);
#595=PLANE('',#5079);
#596=PLANE('',#5080);
#597=PLANE('',#5081);
#598=PLANE('',#5082);
#599=PLANE('',#5083);
#600=PLANE('',#5084);
#601=PLANE('',#5085);
#602=PLANE('',#5086);
#603=PLANE('',#5121);
#604=PLANE('',#5122);
#605=PLANE('',#5124);
#606=PLANE('',#5132);
#607=PLANE('',#5140);
#608=PLANE('',#5141);
#609=PLANE('',#5142);
#610=PLANE('',#5143);
#611=PLANE('',#5144);
#612=PLANE('',#5145);
#613=PLANE('',#5146);
#614=PLANE('',#5147);
#615=PLANE('',#5148);
#616=FACE_OUTER_BOUND('',#873,.T.);
#617=FACE_OUTER_BOUND('',#874,.T.);
#618=FACE_OUTER_BOUND('',#875,.T.);
#619=FACE_OUTER_BOUND('',#876,.T.);
#620=FACE_OUTER_BOUND('',#877,.T.);
#621=FACE_OUTER_BOUND('',#878,.T.);
#622=FACE_OUTER_BOUND('',#879,.T.);
#623=FACE_OUTER_BOUND('',#880,.T.);
#624=FACE_OUTER_BOUND('',#881,.T.);
#625=FACE_OUTER_BOUND('',#882,.T.);
#626=FACE_OUTER_BOUND('',#883,.T.);
#627=FACE_OUTER_BOUND('',#884,.T.);
#628=FACE_OUTER_BOUND('',#885,.T.);
#629=FACE_OUTER_BOUND('',#886,.T.);
#630=FACE_OUTER_BOUND('',#887,.T.);
#631=FACE_OUTER_BOUND('',#888,.T.);
#632=FACE_OUTER_BOUND('',#889,.T.);
#633=FACE_OUTER_BOUND('',#902,.T.);
#634=FACE_OUTER_BOUND('',#915,.T.);
#635=FACE_OUTER_BOUND('',#916,.T.);
#636=FACE_OUTER_BOUND('',#918,.T.);
#637=FACE_OUTER_BOUND('',#919,.T.);
#638=FACE_OUTER_BOUND('',#921,.T.);
#639=FACE_OUTER_BOUND('',#922,.T.);
#640=FACE_OUTER_BOUND('',#923,.T.);
#641=FACE_OUTER_BOUND('',#924,.T.);
#642=FACE_OUTER_BOUND('',#925,.T.);
#643=FACE_OUTER_BOUND('',#926,.T.);
#644=FACE_OUTER_BOUND('',#927,.T.);
#645=FACE_OUTER_BOUND('',#930,.T.);
#646=FACE_OUTER_BOUND('',#933,.T.);
#647=FACE_OUTER_BOUND('',#934,.T.);
#648=FACE_OUTER_BOUND('',#935,.T.);
#649=FACE_OUTER_BOUND('',#936,.T.);
#650=FACE_OUTER_BOUND('',#937,.T.);
#651=FACE_OUTER_BOUND('',#938,.T.);
#652=FACE_OUTER_BOUND('',#939,.T.);
#653=FACE_OUTER_BOUND('',#940,.T.);
#654=FACE_OUTER_BOUND('',#942,.T.);
#655=FACE_OUTER_BOUND('',#943,.T.);
#656=FACE_OUTER_BOUND('',#945,.T.);
#657=FACE_OUTER_BOUND('',#946,.T.);
#658=FACE_OUTER_BOUND('',#947,.T.);
#659=FACE_OUTER_BOUND('',#948,.T.);
#660=FACE_OUTER_BOUND('',#949,.T.);
#661=FACE_OUTER_BOUND('',#950,.T.);
#662=FACE_OUTER_BOUND('',#951,.T.);
#663=FACE_OUTER_BOUND('',#954,.T.);
#664=FACE_OUTER_BOUND('',#957,.T.);
#665=FACE_OUTER_BOUND('',#958,.T.);
#666=FACE_OUTER_BOUND('',#959,.T.);
#667=FACE_OUTER_BOUND('',#960,.T.);
#668=FACE_OUTER_BOUND('',#961,.T.);
#669=FACE_OUTER_BOUND('',#962,.T.);
#670=FACE_OUTER_BOUND('',#963,.T.);
#671=FACE_OUTER_BOUND('',#964,.T.);
#672=FACE_OUTER_BOUND('',#965,.T.);
#673=FACE_OUTER_BOUND('',#966,.T.);
#674=FACE_OUTER_BOUND('',#967,.T.);
#675=FACE_OUTER_BOUND('',#968,.T.);
#676=FACE_OUTER_BOUND('',#969,.T.);
#677=FACE_OUTER_BOUND('',#970,.T.);
#678=FACE_OUTER_BOUND('',#971,.T.);
#679=FACE_OUTER_BOUND('',#972,.T.);
#680=FACE_OUTER_BOUND('',#974,.T.);
#681=FACE_OUTER_BOUND('',#976,.T.);
#682=FACE_OUTER_BOUND('',#978,.T.);
#683=FACE_OUTER_BOUND('',#979,.T.);
#684=FACE_OUTER_BOUND('',#980,.T.);
#685=FACE_OUTER_BOUND('',#981,.T.);
#686=FACE_OUTER_BOUND('',#982,.T.);
#687=FACE_OUTER_BOUND('',#983,.T.);
#688=FACE_OUTER_BOUND('',#985,.T.);
#689=FACE_OUTER_BOUND('',#986,.T.);
#690=FACE_OUTER_BOUND('',#989,.T.);
#691=FACE_OUTER_BOUND('',#990,.T.);
#692=FACE_OUTER_BOUND('',#992,.T.);
#693=FACE_OUTER_BOUND('',#993,.T.);
#694=FACE_OUTER_BOUND('',#995,.T.);
#695=FACE_OUTER_BOUND('',#996,.T.);
#696=FACE_OUTER_BOUND('',#998,.T.);
#697=FACE_OUTER_BOUND('',#999,.T.);
#698=FACE_OUTER_BOUND('',#1001,.T.);
#699=FACE_OUTER_BOUND('',#1002,.T.);
#700=FACE_OUTER_BOUND('',#1003,.T.);
#701=FACE_OUTER_BOUND('',#1004,.T.);
#702=FACE_OUTER_BOUND('',#1005,.T.);
#703=FACE_OUTER_BOUND('',#1006,.T.);
#704=FACE_OUTER_BOUND('',#1007,.T.);
#705=FACE_OUTER_BOUND('',#1008,.T.);
#706=FACE_OUTER_BOUND('',#1009,.T.);
#707=FACE_OUTER_BOUND('',#1010,.T.);
#708=FACE_OUTER_BOUND('',#1011,.T.);
#709=FACE_OUTER_BOUND('',#1012,.T.);
#710=FACE_OUTER_BOUND('',#1013,.T.);
#711=FACE_OUTER_BOUND('',#1014,.T.);
#712=FACE_OUTER_BOUND('',#1016,.T.);
#713=FACE_OUTER_BOUND('',#1017,.T.);
#714=FACE_OUTER_BOUND('',#1018,.T.);
#715=FACE_OUTER_BOUND('',#1019,.T.);
#716=FACE_OUTER_BOUND('',#1020,.T.);
#717=FACE_OUTER_BOUND('',#1021,.T.);
#718=FACE_OUTER_BOUND('',#1022,.T.);
#719=FACE_OUTER_BOUND('',#1023,.T.);
#720=FACE_OUTER_BOUND('',#1024,.T.);
#721=FACE_OUTER_BOUND('',#1025,.T.);
#722=FACE_OUTER_BOUND('',#1026,.T.);
#723=FACE_OUTER_BOUND('',#1027,.T.);
#724=FACE_OUTER_BOUND('',#1028,.T.);
#725=FACE_OUTER_BOUND('',#1029,.T.);
#726=FACE_OUTER_BOUND('',#1030,.T.);
#727=FACE_OUTER_BOUND('',#1031,.T.);
#728=FACE_OUTER_BOUND('',#1032,.T.);
#729=FACE_OUTER_BOUND('',#1033,.T.);
#730=FACE_OUTER_BOUND('',#1034,.T.);
#731=FACE_OUTER_BOUND('',#1035,.T.);
#732=FACE_OUTER_BOUND('',#1036,.T.);
#733=FACE_OUTER_BOUND('',#1037,.T.);
#734=FACE_OUTER_BOUND('',#1038,.T.);
#735=FACE_OUTER_BOUND('',#1039,.T.);
#736=FACE_OUTER_BOUND('',#1040,.T.);
#737=FACE_OUTER_BOUND('',#1041,.T.);
#738=FACE_OUTER_BOUND('',#1042,.T.);
#739=FACE_OUTER_BOUND('',#1043,.T.);
#740=FACE_OUTER_BOUND('',#1044,.T.);
#741=FACE_OUTER_BOUND('',#1045,.T.);
#742=FACE_OUTER_BOUND('',#1052,.T.);
#743=FACE_OUTER_BOUND('',#1053,.T.);
#744=FACE_OUTER_BOUND('',#1060,.T.);
#745=FACE_OUTER_BOUND('',#1065,.T.);
#746=FACE_OUTER_BOUND('',#1066,.T.);
#747=FACE_OUTER_BOUND('',#1067,.T.);
#748=FACE_OUTER_BOUND('',#1068,.T.);
#749=FACE_OUTER_BOUND('',#1070,.T.);
#750=FACE_OUTER_BOUND('',#1072,.T.);
#751=FACE_OUTER_BOUND('',#1073,.T.);
#752=FACE_OUTER_BOUND('',#1074,.T.);
#753=FACE_OUTER_BOUND('',#1076,.T.);
#754=FACE_OUTER_BOUND('',#1078,.T.);
#755=FACE_OUTER_BOUND('',#1079,.T.);
#756=FACE_OUTER_BOUND('',#1080,.T.);
#757=FACE_OUTER_BOUND('',#1081,.T.);
#758=FACE_OUTER_BOUND('',#1082,.T.);
#759=FACE_OUTER_BOUND('',#1083,.T.);
#760=FACE_OUTER_BOUND('',#1084,.T.);
#761=FACE_OUTER_BOUND('',#1085,.T.);
#762=FACE_OUTER_BOUND('',#1092,.T.);
#763=FACE_OUTER_BOUND('',#1093,.T.);
#764=FACE_OUTER_BOUND('',#1100,.T.);
#765=FACE_OUTER_BOUND('',#1101,.T.);
#766=FACE_OUTER_BOUND('',#1102,.T.);
#767=FACE_OUTER_BOUND('',#1103,.T.);
#768=FACE_OUTER_BOUND('',#1104,.T.);
#769=FACE_OUTER_BOUND('',#1105,.T.);
#770=FACE_OUTER_BOUND('',#1106,.T.);
#771=FACE_OUTER_BOUND('',#1107,.T.);
#772=FACE_OUTER_BOUND('',#1108,.T.);
#773=FACE_OUTER_BOUND('',#1109,.T.);
#774=FACE_OUTER_BOUND('',#1116,.T.);
#775=FACE_OUTER_BOUND('',#1117,.T.);
#776=FACE_OUTER_BOUND('',#1124,.T.);
#777=FACE_OUTER_BOUND('',#1125,.T.);
#778=FACE_OUTER_BOUND('',#1126,.T.);
#779=FACE_OUTER_BOUND('',#1127,.T.);
#780=FACE_OUTER_BOUND('',#1128,.T.);
#781=FACE_OUTER_BOUND('',#1129,.T.);
#782=FACE_OUTER_BOUND('',#1130,.T.);
#783=FACE_OUTER_BOUND('',#1131,.T.);
#784=FACE_OUTER_BOUND('',#1132,.T.);
#785=FACE_OUTER_BOUND('',#1133,.T.);
#786=FACE_OUTER_BOUND('',#1134,.T.);
#787=FACE_OUTER_BOUND('',#1135,.T.);
#788=FACE_OUTER_BOUND('',#1141,.T.);
#789=FACE_OUTER_BOUND('',#1147,.T.);
#790=FACE_OUTER_BOUND('',#1148,.T.);
#791=FACE_OUTER_BOUND('',#1149,.T.);
#792=FACE_OUTER_BOUND('',#1151,.T.);
#793=FACE_OUTER_BOUND('',#1153,.T.);
#794=FACE_OUTER_BOUND('',#1154,.T.);
#795=FACE_OUTER_BOUND('',#1155,.T.);
#796=FACE_OUTER_BOUND('',#1156,.T.);
#797=FACE_OUTER_BOUND('',#1157,.T.);
#798=FACE_OUTER_BOUND('',#1158,.T.);
#799=FACE_OUTER_BOUND('',#1160,.T.);
#800=FACE_OUTER_BOUND('',#1161,.T.);
#801=FACE_OUTER_BOUND('',#1163,.T.);
#802=FACE_OUTER_BOUND('',#1164,.T.);
#803=FACE_OUTER_BOUND('',#1166,.T.);
#804=FACE_OUTER_BOUND('',#1167,.T.);
#805=FACE_OUTER_BOUND('',#1169,.T.);
#806=FACE_OUTER_BOUND('',#1170,.T.);
#807=FACE_OUTER_BOUND('',#1172,.T.);
#808=FACE_OUTER_BOUND('',#1173,.T.);
#809=FACE_OUTER_BOUND('',#1175,.T.);
#810=FACE_OUTER_BOUND('',#1177,.T.);
#811=FACE_OUTER_BOUND('',#1178,.T.);
#812=FACE_OUTER_BOUND('',#1179,.T.);
#813=FACE_OUTER_BOUND('',#1180,.T.);
#814=FACE_OUTER_BOUND('',#1181,.T.);
#815=FACE_OUTER_BOUND('',#1183,.T.);
#816=FACE_OUTER_BOUND('',#1185,.T.);
#817=FACE_OUTER_BOUND('',#1187,.T.);
#818=FACE_OUTER_BOUND('',#1189,.T.);
#819=FACE_OUTER_BOUND('',#1190,.T.);
#820=FACE_OUTER_BOUND('',#1191,.T.);
#821=FACE_OUTER_BOUND('',#1192,.T.);
#822=FACE_OUTER_BOUND('',#1193,.T.);
#823=FACE_OUTER_BOUND('',#1195,.T.);
#824=FACE_OUTER_BOUND('',#1196,.T.);
#825=FACE_OUTER_BOUND('',#1197,.T.);
#826=FACE_OUTER_BOUND('',#1198,.T.);
#827=FACE_OUTER_BOUND('',#1199,.T.);
#828=FACE_OUTER_BOUND('',#1200,.T.);
#829=FACE_OUTER_BOUND('',#1201,.T.);
#830=FACE_OUTER_BOUND('',#1202,.T.);
#831=FACE_OUTER_BOUND('',#1203,.T.);
#832=FACE_OUTER_BOUND('',#1204,.T.);
#833=FACE_OUTER_BOUND('',#1205,.T.);
#834=FACE_OUTER_BOUND('',#1206,.T.);
#835=FACE_OUTER_BOUND('',#1207,.T.);
#836=FACE_OUTER_BOUND('',#1208,.T.);
#837=FACE_OUTER_BOUND('',#1209,.T.);
#838=FACE_OUTER_BOUND('',#1210,.T.);
#839=FACE_OUTER_BOUND('',#1211,.T.);
#840=FACE_OUTER_BOUND('',#1213,.T.);
#841=FACE_OUTER_BOUND('',#1214,.T.);
#842=FACE_OUTER_BOUND('',#1215,.T.);
#843=FACE_OUTER_BOUND('',#1216,.T.);
#844=FACE_OUTER_BOUND('',#1217,.T.);
#845=FACE_OUTER_BOUND('',#1218,.T.);
#846=FACE_OUTER_BOUND('',#1219,.T.);
#847=FACE_OUTER_BOUND('',#1220,.T.);
#848=FACE_OUTER_BOUND('',#1221,.T.);
#849=FACE_OUTER_BOUND('',#1222,.T.);
#850=FACE_OUTER_BOUND('',#1223,.T.);
#851=FACE_OUTER_BOUND('',#1224,.T.);
#852=FACE_OUTER_BOUND('',#1225,.T.);
#853=FACE_OUTER_BOUND('',#1226,.T.);
#854=FACE_OUTER_BOUND('',#1227,.T.);
#855=FACE_OUTER_BOUND('',#1229,.T.);
#856=FACE_OUTER_BOUND('',#1231,.T.);
#857=FACE_OUTER_BOUND('',#1232,.T.);
#858=FACE_OUTER_BOUND('',#1233,.T.);
#859=FACE_OUTER_BOUND('',#1234,.T.);
#860=FACE_OUTER_BOUND('',#1235,.T.);
#861=FACE_OUTER_BOUND('',#1237,.T.);
#862=FACE_OUTER_BOUND('',#1238,.T.);
#863=FACE_OUTER_BOUND('',#1239,.T.);
#864=FACE_OUTER_BOUND('',#1240,.T.);
#865=FACE_OUTER_BOUND('',#1241,.T.);
#866=FACE_OUTER_BOUND('',#1242,.T.);
#867=FACE_OUTER_BOUND('',#1243,.T.);
#868=FACE_OUTER_BOUND('',#1244,.T.);
#869=FACE_OUTER_BOUND('',#1245,.T.);
#870=FACE_OUTER_BOUND('',#1246,.T.);
#871=FACE_OUTER_BOUND('',#1247,.T.);
#872=FACE_OUTER_BOUND('',#1248,.T.);
#873=EDGE_LOOP('',(#2994,#2995,#2996,#2997));
#874=EDGE_LOOP('',(#2998,#2999,#3000,#3001));
#875=EDGE_LOOP('',(#3002,#3003,#3004,#3005));
#876=EDGE_LOOP('',(#3006,#3007,#3008,#3009));
#877=EDGE_LOOP('',(#3010,#3011,#3012,#3013));
#878=EDGE_LOOP('',(#3014,#3015,#3016,#3017));
#879=EDGE_LOOP('',(#3018,#3019,#3020,#3021));
#880=EDGE_LOOP('',(#3022,#3023,#3024,#3025));
#881=EDGE_LOOP('',(#3026,#3027,#3028,#3029));
#882=EDGE_LOOP('',(#3030,#3031,#3032,#3033));
#883=EDGE_LOOP('',(#3034,#3035,#3036,#3037));
#884=EDGE_LOOP('',(#3038,#3039,#3040,#3041));
#885=EDGE_LOOP('',(#3042,#3043,#3044,#3045));
#886=EDGE_LOOP('',(#3046,#3047,#3048,#3049));
#887=EDGE_LOOP('',(#3050,#3051,#3052,#3053));
#888=EDGE_LOOP('',(#3054,#3055,#3056,#3057));
#889=EDGE_LOOP('',(#3058,#3059,#3060,#3061));
#890=EDGE_LOOP('',(#3062));
#891=EDGE_LOOP('',(#3063));
#892=EDGE_LOOP('',(#3064));
#893=EDGE_LOOP('',(#3065));
#894=EDGE_LOOP('',(#3066));
#895=EDGE_LOOP('',(#3067));
#896=EDGE_LOOP('',(#3068));
#897=EDGE_LOOP('',(#3069));
#898=EDGE_LOOP('',(#3070));
#899=EDGE_LOOP('',(#3071));
#900=EDGE_LOOP('',(#3072));
#901=EDGE_LOOP('',(#3073));
#902=EDGE_LOOP('',(#3074,#3075,#3076,#3077));
#903=EDGE_LOOP('',(#3078));
#904=EDGE_LOOP('',(#3079));
#905=EDGE_LOOP('',(#3080));
#906=EDGE_LOOP('',(#3081));
#907=EDGE_LOOP('',(#3082));
#908=EDGE_LOOP('',(#3083));
#909=EDGE_LOOP('',(#3084));
#910=EDGE_LOOP('',(#3085));
#911=EDGE_LOOP('',(#3086));
#912=EDGE_LOOP('',(#3087));
#913=EDGE_LOOP('',(#3088));
#914=EDGE_LOOP('',(#3089));
#915=EDGE_LOOP('',(#3090,#3091,#3092,#3093));
#916=EDGE_LOOP('',(#3094));
#917=EDGE_LOOP('',(#3095));
#918=EDGE_LOOP('',(#3096,#3097,#3098,#3099));
#919=EDGE_LOOP('',(#3100));
#920=EDGE_LOOP('',(#3101));
#921=EDGE_LOOP('',(#3102,#3103,#3104,#3105));
#922=EDGE_LOOP('',(#3106,#3107,#3108,#3109));
#923=EDGE_LOOP('',(#3110,#3111,#3112,#3113));
#924=EDGE_LOOP('',(#3114,#3115,#3116,#3117));
#925=EDGE_LOOP('',(#3118,#3119,#3120,#3121));
#926=EDGE_LOOP('',(#3122,#3123,#3124,#3125));
#927=EDGE_LOOP('',(#3126,#3127,#3128,#3129));
#928=EDGE_LOOP('',(#3130));
#929=EDGE_LOOP('',(#3131));
#930=EDGE_LOOP('',(#3132,#3133,#3134,#3135));
#931=EDGE_LOOP('',(#3136));
#932=EDGE_LOOP('',(#3137));
#933=EDGE_LOOP('',(#3138,#3139,#3140,#3141));
#934=EDGE_LOOP('',(#3142,#3143,#3144,#3145));
#935=EDGE_LOOP('',(#3146,#3147,#3148,#3149));
#936=EDGE_LOOP('',(#3150,#3151,#3152,#3153));
#937=EDGE_LOOP('',(#3154,#3155,#3156,#3157));
#938=EDGE_LOOP('',(#3158,#3159,#3160,#3161));
#939=EDGE_LOOP('',(#3162,#3163,#3164,#3165));
#940=EDGE_LOOP('',(#3166));
#941=EDGE_LOOP('',(#3167));
#942=EDGE_LOOP('',(#3168,#3169,#3170,#3171));
#943=EDGE_LOOP('',(#3172));
#944=EDGE_LOOP('',(#3173));
#945=EDGE_LOOP('',(#3174,#3175,#3176,#3177));
#946=EDGE_LOOP('',(#3178,#3179,#3180,#3181));
#947=EDGE_LOOP('',(#3182,#3183,#3184,#3185));
#948=EDGE_LOOP('',(#3186,#3187,#3188,#3189));
#949=EDGE_LOOP('',(#3190,#3191,#3192,#3193));
#950=EDGE_LOOP('',(#3194,#3195,#3196,#3197));
#951=EDGE_LOOP('',(#3198,#3199,#3200,#3201));
#952=EDGE_LOOP('',(#3202));
#953=EDGE_LOOP('',(#3203));
#954=EDGE_LOOP('',(#3204,#3205,#3206,#3207));
#955=EDGE_LOOP('',(#3208));
#956=EDGE_LOOP('',(#3209));
#957=EDGE_LOOP('',(#3210,#3211,#3212,#3213));
#958=EDGE_LOOP('',(#3214,#3215,#3216,#3217));
#959=EDGE_LOOP('',(#3218,#3219,#3220,#3221));
#960=EDGE_LOOP('',(#3222,#3223,#3224,#3225));
#961=EDGE_LOOP('',(#3226,#3227,#3228,#3229));
#962=EDGE_LOOP('',(#3230,#3231,#3232,#3233));
#963=EDGE_LOOP('',(#3234,#3235,#3236,#3237));
#964=EDGE_LOOP('',(#3238,#3239,#3240,#3241));
#965=EDGE_LOOP('',(#3242));
#966=EDGE_LOOP('',(#3243,#3244,#3245,#3246));
#967=EDGE_LOOP('',(#3247));
#968=EDGE_LOOP('',(#3248,#3249));
#969=EDGE_LOOP('',(#3250,#3251,#3252,#3253));
#970=EDGE_LOOP('',(#3254,#3255,#3256,#3257));
#971=EDGE_LOOP('',(#3258,#3259));
#972=EDGE_LOOP('',(#3260,#3261,#3262,#3263,#3264,#3265));
#973=EDGE_LOOP('',(#3266));
#974=EDGE_LOOP('',(#3267,#3268,#3269,#3270,#3271,#3272,#3273,#3274));
#975=EDGE_LOOP('',(#3275));
#976=EDGE_LOOP('',(#3276,#3277,#3278,#3279,#3280,#3281));
#977=EDGE_LOOP('',(#3282));
#978=EDGE_LOOP('',(#3283,#3284,#3285,#3286));
#979=EDGE_LOOP('',(#3287,#3288,#3289,#3290));
#980=EDGE_LOOP('',(#3291,#3292,#3293,#3294));
#981=EDGE_LOOP('',(#3295,#3296,#3297,#3298));
#982=EDGE_LOOP('',(#3299,#3300,#3301,#3302));
#983=EDGE_LOOP('',(#3303,#3304,#3305,#3306,#3307,#3308,#3309,#3310,#3311,
#3312,#3313,#3314));
#984=EDGE_LOOP('',(#3315));
#985=EDGE_LOOP('',(#3316,#3317,#3318,#3319));
#986=EDGE_LOOP('',(#3320,#3321,#3322,#3323));
#987=EDGE_LOOP('',(#3324));
#988=EDGE_LOOP('',(#3325));
#989=EDGE_LOOP('',(#3326,#3327,#3328,#3329));
#990=EDGE_LOOP('',(#3330,#3331,#3332,#3333,#3334,#3335,#3336,#3337));
#991=EDGE_LOOP('',(#3338));
#992=EDGE_LOOP('',(#3339,#3340,#3341,#3342));
#993=EDGE_LOOP('',(#3343,#3344,#3345,#3346));
#994=EDGE_LOOP('',(#3347));
#995=EDGE_LOOP('',(#3348,#3349,#3350,#3351));
#996=EDGE_LOOP('',(#3352,#3353,#3354,#3355));
#997=EDGE_LOOP('',(#3356));
#998=EDGE_LOOP('',(#3357,#3358,#3359,#3360));
#999=EDGE_LOOP('',(#3361,#3362,#3363,#3364,#3365,#3366,#3367,#3368,#3369,
#3370,#3371,#3372));
#1000=EDGE_LOOP('',(#3373));
#1001=EDGE_LOOP('',(#3374,#3375,#3376,#3377));
#1002=EDGE_LOOP('',(#3378,#3379,#3380,#3381));
#1003=EDGE_LOOP('',(#3382,#3383,#3384,#3385));
#1004=EDGE_LOOP('',(#3386,#3387,#3388,#3389));
#1005=EDGE_LOOP('',(#3390,#3391,#3392,#3393));
#1006=EDGE_LOOP('',(#3394,#3395,#3396,#3397));
#1007=EDGE_LOOP('',(#3398,#3399,#3400,#3401,#3402,#3403));
#1008=EDGE_LOOP('',(#3404,#3405,#3406,#3407,#3408,#3409));
#1009=EDGE_LOOP('',(#3410));
#1010=EDGE_LOOP('',(#3411));
#1011=EDGE_LOOP('',(#3412,#3413,#3414,#3415));
#1012=EDGE_LOOP('',(#3416,#3417,#3418,#3419));
#1013=EDGE_LOOP('',(#3420,#3421,#3422,#3423));
#1014=EDGE_LOOP('',(#3424));
#1015=EDGE_LOOP('',(#3425));
#1016=EDGE_LOOP('',(#3426,#3427,#3428,#3429));
#1017=EDGE_LOOP('',(#3430,#3431,#3432,#3433));
#1018=EDGE_LOOP('',(#3434,#3435,#3436,#3437));
#1019=EDGE_LOOP('',(#3438));
#1020=EDGE_LOOP('',(#3439,#3440,#3441,#3442));
#1021=EDGE_LOOP('',(#3443));
#1022=EDGE_LOOP('',(#3444,#3445,#3446,#3447));
#1023=EDGE_LOOP('',(#3448));
#1024=EDGE_LOOP('',(#3449,#3450,#3451,#3452));
#1025=EDGE_LOOP('',(#3453));
#1026=EDGE_LOOP('',(#3454,#3455,#3456,#3457));
#1027=EDGE_LOOP('',(#3458));
#1028=EDGE_LOOP('',(#3459,#3460,#3461,#3462));
#1029=EDGE_LOOP('',(#3463));
#1030=EDGE_LOOP('',(#3464,#3465,#3466,#3467));
#1031=EDGE_LOOP('',(#3468));
#1032=EDGE_LOOP('',(#3469,#3470,#3471,#3472));
#1033=EDGE_LOOP('',(#3473));
#1034=EDGE_LOOP('',(#3474,#3475,#3476,#3477));
#1035=EDGE_LOOP('',(#3478));
#1036=EDGE_LOOP('',(#3479,#3480,#3481,#3482));
#1037=EDGE_LOOP('',(#3483));
#1038=EDGE_LOOP('',(#3484,#3485,#3486,#3487));
#1039=EDGE_LOOP('',(#3488));
#1040=EDGE_LOOP('',(#3489,#3490,#3491,#3492));
#1041=EDGE_LOOP('',(#3493));
#1042=EDGE_LOOP('',(#3494,#3495,#3496,#3497));
#1043=EDGE_LOOP('',(#3498,#3499,#3500,#3501));
#1044=EDGE_LOOP('',(#3502,#3503,#3504,#3505));
#1045=EDGE_LOOP('',(#3506,#3507,#3508,#3509));
#1046=EDGE_LOOP('',(#3510));
#1047=EDGE_LOOP('',(#3511));
#1048=EDGE_LOOP('',(#3512));
#1049=EDGE_LOOP('',(#3513));
#1050=EDGE_LOOP('',(#3514));
#1051=EDGE_LOOP('',(#3515));
#1052=EDGE_LOOP('',(#3516,#3517,#3518,#3519));
#1053=EDGE_LOOP('',(#3520,#3521,#3522,#3523));
#1054=EDGE_LOOP('',(#3524));
#1055=EDGE_LOOP('',(#3525));
#1056=EDGE_LOOP('',(#3526));
#1057=EDGE_LOOP('',(#3527));
#1058=EDGE_LOOP('',(#3528));
#1059=EDGE_LOOP('',(#3529));
#1060=EDGE_LOOP('',(#3530,#3531,#3532,#3533));
#1061=EDGE_LOOP('',(#3534));
#1062=EDGE_LOOP('',(#3535));
#1063=EDGE_LOOP('',(#3536));
#1064=EDGE_LOOP('',(#3537));
#1065=EDGE_LOOP('',(#3538,#3539,#3540,#3541));
#1066=EDGE_LOOP('',(#3542,#3543,#3544,#3545));
#1067=EDGE_LOOP('',(#3546,#3547,#3548,#3549));
#1068=EDGE_LOOP('',(#3550));
#1069=EDGE_LOOP('',(#3551));
#1070=EDGE_LOOP('',(#3552));
#1071=EDGE_LOOP('',(#3553));
#1072=EDGE_LOOP('',(#3554,#3555,#3556,#3557));
#1073=EDGE_LOOP('',(#3558,#3559,#3560,#3561));
#1074=EDGE_LOOP('',(#3562));
#1075=EDGE_LOOP('',(#3563));
#1076=EDGE_LOOP('',(#3564));
#1077=EDGE_LOOP('',(#3565));
#1078=EDGE_LOOP('',(#3566,#3567,#3568,#3569));
#1079=EDGE_LOOP('',(#3570,#3571,#3572,#3573));
#1080=EDGE_LOOP('',(#3574,#3575,#3576,#3577));
#1081=EDGE_LOOP('',(#3578,#3579,#3580,#3581));
#1082=EDGE_LOOP('',(#3582,#3583,#3584,#3585));
#1083=EDGE_LOOP('',(#3586,#3587,#3588,#3589));
#1084=EDGE_LOOP('',(#3590,#3591,#3592,#3593));
#1085=EDGE_LOOP('',(#3594,#3595,#3596,#3597));
#1086=EDGE_LOOP('',(#3598));
#1087=EDGE_LOOP('',(#3599));
#1088=EDGE_LOOP('',(#3600));
#1089=EDGE_LOOP('',(#3601));
#1090=EDGE_LOOP('',(#3602));
#1091=EDGE_LOOP('',(#3603));
#1092=EDGE_LOOP('',(#3604,#3605,#3606,#3607));
#1093=EDGE_LOOP('',(#3608,#3609,#3610,#3611));
#1094=EDGE_LOOP('',(#3612));
#1095=EDGE_LOOP('',(#3613));
#1096=EDGE_LOOP('',(#3614));
#1097=EDGE_LOOP('',(#3615));
#1098=EDGE_LOOP('',(#3616));
#1099=EDGE_LOOP('',(#3617));
#1100=EDGE_LOOP('',(#3618,#3619,#3620,#3621));
#1101=EDGE_LOOP('',(#3622,#3623,#3624,#3625));
#1102=EDGE_LOOP('',(#3626,#3627,#3628,#3629));
#1103=EDGE_LOOP('',(#3630,#3631,#3632,#3633));
#1104=EDGE_LOOP('',(#3634,#3635,#3636,#3637));
#1105=EDGE_LOOP('',(#3638,#3639,#3640,#3641));
#1106=EDGE_LOOP('',(#3642,#3643,#3644,#3645));
#1107=EDGE_LOOP('',(#3646,#3647,#3648,#3649));
#1108=EDGE_LOOP('',(#3650,#3651,#3652,#3653));
#1109=EDGE_LOOP('',(#3654,#3655,#3656,#3657));
#1110=EDGE_LOOP('',(#3658));
#1111=EDGE_LOOP('',(#3659));
#1112=EDGE_LOOP('',(#3660));
#1113=EDGE_LOOP('',(#3661));
#1114=EDGE_LOOP('',(#3662));
#1115=EDGE_LOOP('',(#3663));
#1116=EDGE_LOOP('',(#3664,#3665,#3666,#3667));
#1117=EDGE_LOOP('',(#3668,#3669,#3670,#3671));
#1118=EDGE_LOOP('',(#3672));
#1119=EDGE_LOOP('',(#3673));
#1120=EDGE_LOOP('',(#3674));
#1121=EDGE_LOOP('',(#3675));
#1122=EDGE_LOOP('',(#3676));
#1123=EDGE_LOOP('',(#3677));
#1124=EDGE_LOOP('',(#3678,#3679,#3680,#3681));
#1125=EDGE_LOOP('',(#3682,#3683,#3684,#3685));
#1126=EDGE_LOOP('',(#3686,#3687,#3688,#3689));
#1127=EDGE_LOOP('',(#3690,#3691,#3692,#3693));
#1128=EDGE_LOOP('',(#3694,#3695,#3696,#3697));
#1129=EDGE_LOOP('',(#3698,#3699,#3700,#3701));
#1130=EDGE_LOOP('',(#3702,#3703,#3704,#3705));
#1131=EDGE_LOOP('',(#3706,#3707,#3708,#3709));
#1132=EDGE_LOOP('',(#3710,#3711,#3712,#3713));
#1133=EDGE_LOOP('',(#3714,#3715,#3716,#3717));
#1134=EDGE_LOOP('',(#3718,#3719,#3720,#3721));
#1135=EDGE_LOOP('',(#3722,#3723,#3724,#3725));
#1136=EDGE_LOOP('',(#3726));
#1137=EDGE_LOOP('',(#3727));
#1138=EDGE_LOOP('',(#3728));
#1139=EDGE_LOOP('',(#3729));
#1140=EDGE_LOOP('',(#3730));
#1141=EDGE_LOOP('',(#3731,#3732,#3733,#3734));
#1142=EDGE_LOOP('',(#3735));
#1143=EDGE_LOOP('',(#3736));
#1144=EDGE_LOOP('',(#3737));
#1145=EDGE_LOOP('',(#3738));
#1146=EDGE_LOOP('',(#3739));
#1147=EDGE_LOOP('',(#3740,#3741,#3742,#3743));
#1148=EDGE_LOOP('',(#3744,#3745,#3746,#3747));
#1149=EDGE_LOOP('',(#3748));
#1150=EDGE_LOOP('',(#3749));
#1151=EDGE_LOOP('',(#3750));
#1152=EDGE_LOOP('',(#3751));
#1153=EDGE_LOOP('',(#3752,#3753,#3754,#3755));
#1154=EDGE_LOOP('',(#3756,#3757,#3758,#3759));
#1155=EDGE_LOOP('',(#3760,#3761,#3762,#3763));
#1156=EDGE_LOOP('',(#3764,#3765,#3766,#3767));
#1157=EDGE_LOOP('',(#3768,#3769,#3770,#3771));
#1158=EDGE_LOOP('',(#3772));
#1159=EDGE_LOOP('',(#3773));
#1160=EDGE_LOOP('',(#3774,#3775,#3776,#3777));
#1161=EDGE_LOOP('',(#3778));
#1162=EDGE_LOOP('',(#3779));
#1163=EDGE_LOOP('',(#3780,#3781,#3782,#3783));
#1164=EDGE_LOOP('',(#3784));
#1165=EDGE_LOOP('',(#3785));
#1166=EDGE_LOOP('',(#3786,#3787,#3788,#3789));
#1167=EDGE_LOOP('',(#3790));
#1168=EDGE_LOOP('',(#3791));
#1169=EDGE_LOOP('',(#3792,#3793,#3794,#3795));
#1170=EDGE_LOOP('',(#3796));
#1171=EDGE_LOOP('',(#3797));
#1172=EDGE_LOOP('',(#3798,#3799,#3800,#3801));
#1173=EDGE_LOOP('',(#3802));
#1174=EDGE_LOOP('',(#3803));
#1175=EDGE_LOOP('',(#3804,#3805,#3806,#3807));
#1176=EDGE_LOOP('',(#3808,#3809,#3810,#3811));
#1177=EDGE_LOOP('',(#3812,#3813,#3814,#3815));
#1178=EDGE_LOOP('',(#3816,#3817,#3818,#3819));
#1179=EDGE_LOOP('',(#3820,#3821,#3822,#3823));
#1180=EDGE_LOOP('',(#3824,#3825,#3826,#3827));
#1181=EDGE_LOOP('',(#3828));
#1182=EDGE_LOOP('',(#3829));
#1183=EDGE_LOOP('',(#3830,#3831,#3832,#3833));
#1184=EDGE_LOOP('',(#3834,#3835,#3836,#3837));
#1185=EDGE_LOOP('',(#3838));
#1186=EDGE_LOOP('',(#3839));
#1187=EDGE_LOOP('',(#3840,#3841,#3842,#3843));
#1188=EDGE_LOOP('',(#3844,#3845,#3846,#3847));
#1189=EDGE_LOOP('',(#3848));
#1190=EDGE_LOOP('',(#3849,#3850,#3851,#3852));
#1191=EDGE_LOOP('',(#3853,#3854,#3855,#3856));
#1192=EDGE_LOOP('',(#3857,#3858,#3859,#3860));
#1193=EDGE_LOOP('',(#3861));
#1194=EDGE_LOOP('',(#3862));
#1195=EDGE_LOOP('',(#3863,#3864,#3865,#3866));
#1196=EDGE_LOOP('',(#3867,#3868,#3869,#3870));
#1197=EDGE_LOOP('',(#3871,#3872,#3873,#3874));
#1198=EDGE_LOOP('',(#3875));
#1199=EDGE_LOOP('',(#3876,#3877,#3878,#3879));
#1200=EDGE_LOOP('',(#3880,#3881,#3882,#3883));
#1201=EDGE_LOOP('',(#3884,#3885,#3886,#3887));
#1202=EDGE_LOOP('',(#3888,#3889,#3890,#3891));
#1203=EDGE_LOOP('',(#3892,#3893,#3894,#3895));
#1204=EDGE_LOOP('',(#3896,#3897,#3898,#3899));
#1205=EDGE_LOOP('',(#3900,#3901,#3902,#3903,#3904,#3905));
#1206=EDGE_LOOP('',(#3906,#3907,#3908,#3909,#3910,#3911));
#1207=EDGE_LOOP('',(#3912));
#1208=EDGE_LOOP('',(#3913,#3914,#3915,#3916));
#1209=EDGE_LOOP('',(#3917,#3918,#3919,#3920));
#1210=EDGE_LOOP('',(#3921,#3922,#3923,#3924));
#1211=EDGE_LOOP('',(#3925));
#1212=EDGE_LOOP('',(#3926));
#1213=EDGE_LOOP('',(#3927,#3928,#3929,#3930));
#1214=EDGE_LOOP('',(#3931,#3932,#3933,#3934));
#1215=EDGE_LOOP('',(#3935,#3936,#3937,#3938));
#1216=EDGE_LOOP('',(#3939));
#1217=EDGE_LOOP('',(#3940,#3941,#3942,#3943));
#1218=EDGE_LOOP('',(#3944,#3945,#3946,#3947));
#1219=EDGE_LOOP('',(#3948,#3949,#3950,#3951));
#1220=EDGE_LOOP('',(#3952,#3953,#3954,#3955));
#1221=EDGE_LOOP('',(#3956,#3957,#3958,#3959));
#1222=EDGE_LOOP('',(#3960,#3961,#3962,#3963));
#1223=EDGE_LOOP('',(#3964,#3965,#3966,#3967,#3968,#3969));
#1224=EDGE_LOOP('',(#3970,#3971,#3972,#3973,#3974,#3975));
#1225=EDGE_LOOP('',(#3976,#3977,#3978,#3979));
#1226=EDGE_LOOP('',(#3980,#3981,#3982,#3983));
#1227=EDGE_LOOP('',(#3984));
#1228=EDGE_LOOP('',(#3985));
#1229=EDGE_LOOP('',(#3986));
#1230=EDGE_LOOP('',(#3987));
#1231=EDGE_LOOP('',(#3988));
#1232=EDGE_LOOP('',(#3989,#3990,#3991,#3992));
#1233=EDGE_LOOP('',(#3993,#3994,#3995,#3996));
#1234=EDGE_LOOP('',(#3997,#3998,#3999,#4000));
#1235=EDGE_LOOP('',(#4001));
#1236=EDGE_LOOP('',(#4002));
#1237=EDGE_LOOP('',(#4003,#4004,#4005,#4006));
#1238=EDGE_LOOP('',(#4007,#4008,#4009,#4010));
#1239=EDGE_LOOP('',(#4011,#4012,#4013,#4014));
#1240=EDGE_LOOP('',(#4015));
#1241=EDGE_LOOP('',(#4016,#4017,#4018,#4019));
#1242=EDGE_LOOP('',(#4020,#4021,#4022,#4023));
#1243=EDGE_LOOP('',(#4024,#4025,#4026,#4027));
#1244=EDGE_LOOP('',(#4028,#4029,#4030,#4031));
#1245=EDGE_LOOP('',(#4032,#4033,#4034,#4035));
#1246=EDGE_LOOP('',(#4036,#4037,#4038,#4039));
#1247=EDGE_LOOP('',(#4040,#4041,#4042,#4043,#4044,#4045));
#1248=EDGE_LOOP('',(#4046,#4047,#4048,#4049,#4050,#4051));
#1249=LINE('',#6577,#1589);
#1250=LINE('',#6583,#1590);
#1251=LINE('',#6589,#1591);
#1252=LINE('',#6595,#1592);
#1253=LINE('',#6601,#1593);
#1254=LINE('',#6607,#1594);
#1255=LINE('',#6613,#1595);
#1256=LINE('',#6619,#1596);
#1257=LINE('',#6625,#1597);
#1258=LINE('',#6631,#1598);
#1259=LINE('',#6637,#1599);
#1260=LINE('',#6643,#1600);
#1261=LINE('',#6648,#1601);
#1262=LINE('',#6650,#1602);
#1263=LINE('',#6652,#1603);
#1264=LINE('',#6653,#1604);
#1265=LINE('',#6656,#1605);
#1266=LINE('',#6658,#1606);
#1267=LINE('',#6659,#1607);
#1268=LINE('',#6662,#1608);
#1269=LINE('',#6664,#1609);
#1270=LINE('',#6665,#1610);
#1271=LINE('',#6667,#1611);
#1272=LINE('',#6668,#1612);
#1273=LINE('',#6676,#1613);
#1274=LINE('',#6685,#1614);
#1275=LINE('',#6693,#1615);
#1276=LINE('',#6697,#1616);
#1277=LINE('',#6701,#1617);
#1278=LINE('',#6703,#1618);
#1279=LINE('',#6705,#1619);
#1280=LINE('',#6706,#1620);
#1281=LINE('',#6709,#1621);
#1282=LINE('',#6711,#1622);
#1283=LINE('',#6712,#1623);
#1284=LINE('',#6715,#1624);
#1285=LINE('',#6717,#1625);
#1286=LINE('',#6718,#1626);
#1287=LINE('',#6720,#1627);
#1288=LINE('',#6721,#1628);
#1289=LINE('',#6728,#1629);
#1290=LINE('',#6730,#1630);
#1291=LINE('',#6732,#1631);
#1292=LINE('',#6733,#1632);
#1293=LINE('',#6736,#1633);
#1294=LINE('',#6738,#1634);
#1295=LINE('',#6739,#1635);
#1296=LINE('',#6742,#1636);
#1297=LINE('',#6744,#1637);
#1298=LINE('',#6745,#1638);
#1299=LINE('',#6747,#1639);
#1300=LINE('',#6748,#1640);
#1301=LINE('',#6756,#1641);
#1302=LINE('',#6765,#1642);
#1303=LINE('',#6773,#1643);
#1304=LINE('',#6777,#1644);
#1305=LINE('',#6781,#1645);
#1306=LINE('',#6783,#1646);
#1307=LINE('',#6785,#1647);
#1308=LINE('',#6786,#1648);
#1309=LINE('',#6789,#1649);
#1310=LINE('',#6791,#1650);
#1311=LINE('',#6792,#1651);
#1312=LINE('',#6795,#1652);
#1313=LINE('',#6797,#1653);
#1314=LINE('',#6798,#1654);
#1315=LINE('',#6800,#1655);
#1316=LINE('',#6801,#1656);
#1317=LINE('',#6808,#1657);
#1318=LINE('',#6810,#1658);
#1319=LINE('',#6812,#1659);
#1320=LINE('',#6813,#1660);
#1321=LINE('',#6816,#1661);
#1322=LINE('',#6818,#1662);
#1323=LINE('',#6819,#1663);
#1324=LINE('',#6822,#1664);
#1325=LINE('',#6824,#1665);
#1326=LINE('',#6825,#1666);
#1327=LINE('',#6827,#1667);
#1328=LINE('',#6828,#1668);
#1329=LINE('',#6836,#1669);
#1330=LINE('',#6841,#1670);
#1331=LINE('',#6846,#1671);
#1332=LINE('',#6852,#1672);
#1333=LINE('',#6856,#1673);
#1334=LINE('',#6859,#1674);
#1335=LINE('',#6863,#1675);
#1336=LINE('',#6867,#1676);
#1337=LINE('',#6870,#1677);
#1338=LINE('',#6873,#1678);
#1339=LINE('',#6875,#1679);
#1340=LINE('',#6877,#1680);
#1341=LINE('',#6879,#1681);
#1342=LINE('',#6880,#1682);
#1343=LINE('',#6885,#1683);
#1344=LINE('',#6887,#1684);
#1345=LINE('',#6888,#1685);
#1346=LINE('',#6894,#1686);
#1347=LINE('',#6896,#1687);
#1348=LINE('',#6897,#1688);
#1349=LINE('',#6899,#1689);
#1350=LINE('',#6900,#1690);
#1351=LINE('',#6907,#1691);
#1352=LINE('',#6911,#1692);
#1353=LINE('',#6916,#1693);
#1354=LINE('',#6920,#1694);
#1355=LINE('',#6925,#1695);
#1356=LINE('',#6929,#1696);
#1357=LINE('',#6931,#1697);
#1358=LINE('',#6932,#1698);
#1359=LINE('',#6934,#1699);
#1360=LINE('',#6936,#1700);
#1361=LINE('',#6938,#1701);
#1362=LINE('',#6940,#1702);
#1363=LINE('',#6942,#1703);
#1364=LINE('',#6943,#1704);
#1365=LINE('',#6946,#1705);
#1366=LINE('',#6947,#1706);
#1367=LINE('',#6950,#1707);
#1368=LINE('',#6951,#1708);
#1369=LINE('',#6953,#1709);
#1370=LINE('',#6956,#1710);
#1371=LINE('',#6957,#1711);
#1372=LINE('',#6960,#1712);
#1373=LINE('',#6961,#1713);
#1374=LINE('',#6964,#1714);
#1375=LINE('',#6965,#1715);
#1376=LINE('',#6968,#1716);
#1377=LINE('',#6969,#1717);
#1378=LINE('',#6972,#1718);
#1379=LINE('',#6973,#1719);
#1380=LINE('',#6975,#1720);
#1381=LINE('',#6981,#1721);
#1382=LINE('',#6983,#1722);
#1383=LINE('',#6985,#1723);
#1384=LINE('',#6986,#1724);
#1385=LINE('',#6989,#1725);
#1386=LINE('',#6991,#1726);
#1387=LINE('',#6992,#1727);
#1388=LINE('',#6995,#1728);
#1389=LINE('',#6997,#1729);
#1390=LINE('',#6998,#1730);
#1391=LINE('',#7001,#1731);
#1392=LINE('',#7003,#1732);
#1393=LINE('',#7004,#1733);
#1394=LINE('',#7007,#1734);
#1395=LINE('',#7009,#1735);
#1396=LINE('',#7010,#1736);
#1397=LINE('',#7012,#1737);
#1398=LINE('',#7013,#1738);
#1399=LINE('',#7025,#1739);
#1400=LINE('',#7029,#1740);
#1401=LINE('',#7033,#1741);
#1402=LINE('',#7040,#1742);
#1403=LINE('',#7042,#1743);
#1404=LINE('',#7049,#1744);
#1405=LINE('',#7056,#1745);
#1406=LINE('',#7063,#1746);
#1407=LINE('',#7070,#1747);
#1408=LINE('',#7077,#1748);
#1409=LINE('',#7084,#1749);
#1410=LINE('',#7091,#1750);
#1411=LINE('',#7098,#1751);
#1412=LINE('',#7105,#1752);
#1413=LINE('',#7112,#1753);
#1414=LINE('',#7119,#1754);
#1415=LINE('',#7126,#1755);
#1416=LINE('',#7133,#1756);
#1417=LINE('',#7139,#1757);
#1418=LINE('',#7144,#1758);
#1419=LINE('',#7146,#1759);
#1420=LINE('',#7148,#1760);
#1421=LINE('',#7149,#1761);
#1422=LINE('',#7152,#1762);
#1423=LINE('',#7154,#1763);
#1424=LINE('',#7155,#1764);
#1425=LINE('',#7158,#1765);
#1426=LINE('',#7160,#1766);
#1427=LINE('',#7161,#1767);
#1428=LINE('',#7163,#1768);
#1429=LINE('',#7164,#1769);
#1430=LINE('',#7172,#1770);
#1431=LINE('',#7178,#1771);
#1432=LINE('',#7187,#1772);
#1433=LINE('',#7193,#1773);
#1434=LINE('',#7202,#1774);
#1435=LINE('',#7208,#1775);
#1436=LINE('',#7214,#1776);
#1437=LINE('',#7220,#1777);
#1438=LINE('',#7226,#1778);
#1439=LINE('',#7232,#1779);
#1440=LINE('',#7237,#1780);
#1441=LINE('',#7239,#1781);
#1442=LINE('',#7241,#1782);
#1443=LINE('',#7242,#1783);
#1444=LINE('',#7245,#1784);
#1445=LINE('',#7247,#1785);
#1446=LINE('',#7248,#1786);
#1447=LINE('',#7251,#1787);
#1448=LINE('',#7253,#1788);
#1449=LINE('',#7254,#1789);
#1450=LINE('',#7256,#1790);
#1451=LINE('',#7257,#1791);
#1452=LINE('',#7265,#1792);
#1453=LINE('',#7271,#1793);
#1454=LINE('',#7277,#1794);
#1455=LINE('',#7283,#1795);
#1456=LINE('',#7289,#1796);
#1457=LINE('',#7295,#1797);
#1458=LINE('',#7300,#1798);
#1459=LINE('',#7302,#1799);
#1460=LINE('',#7304,#1800);
#1461=LINE('',#7305,#1801);
#1462=LINE('',#7308,#1802);
#1463=LINE('',#7310,#1803);
#1464=LINE('',#7311,#1804);
#1465=LINE('',#7314,#1805);
#1466=LINE('',#7316,#1806);
#1467=LINE('',#7317,#1807);
#1468=LINE('',#7319,#1808);
#1469=LINE('',#7320,#1809);
#1470=LINE('',#7328,#1810);
#1471=LINE('',#7334,#1811);
#1472=LINE('',#7340,#1812);
#1473=LINE('',#7346,#1813);
#1474=LINE('',#7352,#1814);
#1475=LINE('',#7357,#1815);
#1476=LINE('',#7359,#1816);
#1477=LINE('',#7361,#1817);
#1478=LINE('',#7362,#1818);
#1479=LINE('',#7365,#1819);
#1480=LINE('',#7367,#1820);
#1481=LINE('',#7368,#1821);
#1482=LINE('',#7371,#1822);
#1483=LINE('',#7373,#1823);
#1484=LINE('',#7374,#1824);
#1485=LINE('',#7376,#1825);
#1486=LINE('',#7377,#1826);
#1487=LINE('',#7385,#1827);
#1488=LINE('',#7391,#1828);
#1489=LINE('',#7402,#1829);
#1490=LINE('',#7404,#1830);
#1491=LINE('',#7405,#1831);
#1492=LINE('',#7408,#1832);
#1493=LINE('',#7410,#1833);
#1494=LINE('',#7411,#1834);
#1495=LINE('',#7416,#1835);
#1496=LINE('',#7417,#1836);
#1497=LINE('',#7419,#1837);
#1498=LINE('',#7420,#1838);
#1499=LINE('',#7430,#1839);
#1500=LINE('',#7437,#1840);
#1501=LINE('',#7444,#1841);
#1502=LINE('',#7451,#1842);
#1503=LINE('',#7458,#1843);
#1504=LINE('',#7463,#1844);
#1505=LINE('',#7470,#1845);
#1506=LINE('',#7473,#1846);
#1507=LINE('',#7476,#1847);
#1508=LINE('',#7478,#1848);
#1509=LINE('',#7479,#1849);
#1510=LINE('',#7485,#1850);
#1511=LINE('',#7487,#1851);
#1512=LINE('',#7488,#1852);
#1513=LINE('',#7497,#1853);
#1514=LINE('',#7502,#1854);
#1515=LINE('',#7512,#1855);
#1516=LINE('',#7516,#1856);
#1517=LINE('',#7520,#1857);
#1518=LINE('',#7527,#1858);
#1519=LINE('',#7531,#1859);
#1520=LINE('',#7535,#1860);
#1521=LINE('',#7540,#1861);
#1522=LINE('',#7542,#1862);
#1523=LINE('',#7544,#1863);
#1524=LINE('',#7545,#1864);
#1525=LINE('',#7548,#1865);
#1526=LINE('',#7550,#1866);
#1527=LINE('',#7551,#1867);
#1528=LINE('',#7554,#1868);
#1529=LINE('',#7556,#1869);
#1530=LINE('',#7557,#1870);
#1531=LINE('',#7560,#1871);
#1532=LINE('',#7562,#1872);
#1533=LINE('',#7563,#1873);
#1534=LINE('',#7566,#1874);
#1535=LINE('',#7568,#1875);
#1536=LINE('',#7569,#1876);
#1537=LINE('',#7571,#1877);
#1538=LINE('',#7572,#1878);
#1539=LINE('',#7582,#1879);
#1540=LINE('',#7586,#1880);
#1541=LINE('',#7590,#1881);
#1542=LINE('',#7597,#1882);
#1543=LINE('',#7601,#1883);
#1544=LINE('',#7605,#1884);
#1545=LINE('',#7610,#1885);
#1546=LINE('',#7612,#1886);
#1547=LINE('',#7614,#1887);
#1548=LINE('',#7615,#1888);
#1549=LINE('',#7618,#1889);
#1550=LINE('',#7620,#1890);
#1551=LINE('',#7621,#1891);
#1552=LINE('',#7624,#1892);
#1553=LINE('',#7626,#1893);
#1554=LINE('',#7627,#1894);
#1555=LINE('',#7630,#1895);
#1556=LINE('',#7632,#1896);
#1557=LINE('',#7633,#1897);
#1558=LINE('',#7636,#1898);
#1559=LINE('',#7638,#1899);
#1560=LINE('',#7639,#1900);
#1561=LINE('',#7641,#1901);
#1562=LINE('',#7642,#1902);
#1563=LINE('',#7677,#1903);
#1564=LINE('',#7683,#1904);
#1565=LINE('',#7694,#1905);
#1566=LINE('',#7698,#1906);
#1567=LINE('',#7702,#1907);
#1568=LINE('',#7709,#1908);
#1569=LINE('',#7713,#1909);
#1570=LINE('',#7717,#1910);
#1571=LINE('',#7722,#1911);
#1572=LINE('',#7724,#1912);
#1573=LINE('',#7726,#1913);
#1574=LINE('',#7727,#1914);
#1575=LINE('',#7730,#1915);
#1576=LINE('',#7732,#1916);
#1577=LINE('',#7733,#1917);
#1578=LINE('',#7736,#1918);
#1579=LINE('',#7738,#1919);
#1580=LINE('',#7739,#1920);
#1581=LINE('',#7742,#1921);
#1582=LINE('',#7744,#1922);
#1583=LINE('',#7745,#1923);
#1584=LINE('',#7748,#1924);
#1585=LINE('',#7750,#1925);
#1586=LINE('',#7751,#1926);
#1587=LINE('',#7753,#1927);
#1588=LINE('',#7754,#1928);
#1589=VECTOR('',#5186,0.210000000000001);
#1590=VECTOR('',#5193,0.21);
#1591=VECTOR('',#5200,0.21);
#1592=VECTOR('',#5207,0.210000000000001);
#1593=VECTOR('',#5214,0.210000000000001);
#1594=VECTOR('',#5221,0.210000000000001);
#1595=VECTOR('',#5228,0.21);
#1596=VECTOR('',#5235,0.21);
#1597=VECTOR('',#5242,0.21);
#1598=VECTOR('',#5249,0.21);
#1599=VECTOR('',#5256,0.210000000000001);
#1600=VECTOR('',#5263,0.210000000000001);
#1601=VECTOR('',#5268,1.);
#1602=VECTOR('',#5269,1.);
#1603=VECTOR('',#5270,1.);
#1604=VECTOR('',#5271,1.);
#1605=VECTOR('',#5274,1.);
#1606=VECTOR('',#5275,1.);
#1607=VECTOR('',#5276,1.);
#1608=VECTOR('',#5279,1.);
#1609=VECTOR('',#5280,1.);
#1610=VECTOR('',#5281,1.);
#1611=VECTOR('',#5284,1.);
#1612=VECTOR('',#5285,1.);
#1613=VECTOR('',#5296,0.475);
#1614=VECTOR('',#5307,0.475);
#1615=VECTOR('',#5318,0.275);
#1616=VECTOR('',#5323,0.275);
#1617=VECTOR('',#5326,1.);
#1618=VECTOR('',#5327,1.);
#1619=VECTOR('',#5328,1.);
#1620=VECTOR('',#5329,1.);
#1621=VECTOR('',#5332,1.);
#1622=VECTOR('',#5333,1.);
#1623=VECTOR('',#5334,1.);
#1624=VECTOR('',#5337,1.);
#1625=VECTOR('',#5338,1.);
#1626=VECTOR('',#5339,1.);
#1627=VECTOR('',#5342,1.);
#1628=VECTOR('',#5343,1.);
#1629=VECTOR('',#5352,1.);
#1630=VECTOR('',#5353,1.);
#1631=VECTOR('',#5354,1.);
#1632=VECTOR('',#5355,1.);
#1633=VECTOR('',#5358,1.);
#1634=VECTOR('',#5359,1.);
#1635=VECTOR('',#5360,1.);
#1636=VECTOR('',#5363,1.);
#1637=VECTOR('',#5364,1.);
#1638=VECTOR('',#5365,1.);
#1639=VECTOR('',#5368,1.);
#1640=VECTOR('',#5369,1.);
#1641=VECTOR('',#5380,0.475000000000001);
#1642=VECTOR('',#5391,0.475000000000001);
#1643=VECTOR('',#5402,0.274999999999999);
#1644=VECTOR('',#5407,0.274999999999999);
#1645=VECTOR('',#5410,1.);
#1646=VECTOR('',#5411,1.);
#1647=VECTOR('',#5412,1.);
#1648=VECTOR('',#5413,1.);
#1649=VECTOR('',#5416,1.);
#1650=VECTOR('',#5417,1.);
#1651=VECTOR('',#5418,1.);
#1652=VECTOR('',#5421,1.);
#1653=VECTOR('',#5422,1.);
#1654=VECTOR('',#5423,1.);
#1655=VECTOR('',#5426,1.);
#1656=VECTOR('',#5427,1.);
#1657=VECTOR('',#5436,1.);
#1658=VECTOR('',#5437,1.);
#1659=VECTOR('',#5438,1.);
#1660=VECTOR('',#5439,1.);
#1661=VECTOR('',#5442,1.);
#1662=VECTOR('',#5443,1.);
#1663=VECTOR('',#5444,1.);
#1664=VECTOR('',#5447,1.);
#1665=VECTOR('',#5448,1.);
#1666=VECTOR('',#5449,1.);
#1667=VECTOR('',#5452,1.);
#1668=VECTOR('',#5453,1.);
#1669=VECTOR('',#5464,0.55);
#1670=VECTOR('',#5471,0.6);
#1671=VECTOR('',#5478,0.55);
#1672=VECTOR('',#5485,1.);
#1673=VECTOR('',#5490,1.);
#1674=VECTOR('',#5493,1.);
#1675=VECTOR('',#5496,1.);
#1676=VECTOR('',#5499,1.);
#1677=VECTOR('',#5504,1.);
#1678=VECTOR('',#5507,1.);
#1679=VECTOR('',#5508,1.);
#1680=VECTOR('',#5509,1.);
#1681=VECTOR('',#5510,1.);
#1682=VECTOR('',#5511,1.);
#1683=VECTOR('',#5516,1.);
#1684=VECTOR('',#5517,1.);
#1685=VECTOR('',#5518,1.);
#1686=VECTOR('',#5523,1.);
#1687=VECTOR('',#5524,1.);
#1688=VECTOR('',#5525,1.);
#1689=VECTOR('',#5526,1.);
#1690=VECTOR('',#5527,1.);
#1691=VECTOR('',#5534,0.225);
#1692=VECTOR('',#5539,0.165);
#1693=VECTOR('',#5546,0.275);
#1694=VECTOR('',#5551,0.275);
#1695=VECTOR('',#5556,0.6);
#1696=VECTOR('',#5561,1.);
#1697=VECTOR('',#5562,1.);
#1698=VECTOR('',#5563,1.);
#1699=VECTOR('',#5564,1.);
#1700=VECTOR('',#5565,1.);
#1701=VECTOR('',#5566,1.);
#1702=VECTOR('',#5567,1.);
#1703=VECTOR('',#5568,1.);
#1704=VECTOR('',#5569,1.);
#1705=VECTOR('',#5572,1.);
#1706=VECTOR('',#5573,1.);
#1707=VECTOR('',#5576,1.);
#1708=VECTOR('',#5577,1.);
#1709=VECTOR('',#5580,1.);
#1710=VECTOR('',#5583,1.);
#1711=VECTOR('',#5584,1.);
#1712=VECTOR('',#5587,1.);
#1713=VECTOR('',#5588,1.);
#1714=VECTOR('',#5591,1.);
#1715=VECTOR('',#5592,1.);
#1716=VECTOR('',#5595,1.);
#1717=VECTOR('',#5596,1.);
#1718=VECTOR('',#5599,1.);
#1719=VECTOR('',#5600,1.);
#1720=VECTOR('',#5603,1.);
#1721=VECTOR('',#5610,1.);
#1722=VECTOR('',#5611,1.);
#1723=VECTOR('',#5612,1.);
#1724=VECTOR('',#5613,1.);
#1725=VECTOR('',#5616,1.);
#1726=VECTOR('',#5617,1.);
#1727=VECTOR('',#5618,1.);
#1728=VECTOR('',#5621,1.);
#1729=VECTOR('',#5622,1.);
#1730=VECTOR('',#5623,1.);
#1731=VECTOR('',#5626,1.);
#1732=VECTOR('',#5627,1.);
#1733=VECTOR('',#5628,1.);
#1734=VECTOR('',#5631,1.);
#1735=VECTOR('',#5632,1.);
#1736=VECTOR('',#5633,1.);
#1737=VECTOR('',#5636,1.);
#1738=VECTOR('',#5637,1.);
#1739=VECTOR('',#5654,0.4);
#1740=VECTOR('',#5659,0.425);
#1741=VECTOR('',#5664,0.41);
#1742=VECTOR('',#5673,0.26);
#1743=VECTOR('',#5676,0.25);
#1744=VECTOR('',#5685,0.165);
#1745=VECTOR('',#5694,0.165);
#1746=VECTOR('',#5703,0.165);
#1747=VECTOR('',#5712,0.165);
#1748=VECTOR('',#5721,0.165);
#1749=VECTOR('',#5730,0.165);
#1750=VECTOR('',#5739,0.165);
#1751=VECTOR('',#5748,0.165);
#1752=VECTOR('',#5757,0.210000000000001);
#1753=VECTOR('',#5766,0.210000000000001);
#1754=VECTOR('',#5775,0.210000000000001);
#1755=VECTOR('',#5784,0.210000000000001);
#1756=VECTOR('',#5793,1.05);
#1757=VECTOR('',#5800,1.05);
#1758=VECTOR('',#5805,1.);
#1759=VECTOR('',#5806,1.);
#1760=VECTOR('',#5807,1.);
#1761=VECTOR('',#5808,1.);
#1762=VECTOR('',#5811,1.);
#1763=VECTOR('',#5812,1.);
#1764=VECTOR('',#5813,1.);
#1765=VECTOR('',#5816,1.);
#1766=VECTOR('',#5817,1.);
#1767=VECTOR('',#5818,1.);
#1768=VECTOR('',#5821,1.);
#1769=VECTOR('',#5822,1.);
#1770=VECTOR('',#5833,0.7);
#1771=VECTOR('',#5840,1.04);
#1772=VECTOR('',#5853,0.7);
#1773=VECTOR('',#5860,1.04);
#1774=VECTOR('',#5873,0.225);
#1775=VECTOR('',#5880,0.225);
#1776=VECTOR('',#5887,0.225);
#1777=VECTOR('',#5894,0.225);
#1778=VECTOR('',#5901,0.7);
#1779=VECTOR('',#5908,0.7);
#1780=VECTOR('',#5913,1.);
#1781=VECTOR('',#5914,1.);
#1782=VECTOR('',#5915,1.);
#1783=VECTOR('',#5916,1.);
#1784=VECTOR('',#5919,1.);
#1785=VECTOR('',#5920,1.);
#1786=VECTOR('',#5921,1.);
#1787=VECTOR('',#5924,1.);
#1788=VECTOR('',#5925,1.);
#1789=VECTOR('',#5926,1.);
#1790=VECTOR('',#5929,1.);
#1791=VECTOR('',#5930,1.);
#1792=VECTOR('',#5941,0.225);
#1793=VECTOR('',#5948,0.225);
#1794=VECTOR('',#5955,0.225);
#1795=VECTOR('',#5962,0.225);
#1796=VECTOR('',#5969,0.7);
#1797=VECTOR('',#5976,0.7);
#1798=VECTOR('',#5981,1.);
#1799=VECTOR('',#5982,1.);
#1800=VECTOR('',#5983,1.);
#1801=VECTOR('',#5984,1.);
#1802=VECTOR('',#5987,1.);
#1803=VECTOR('',#5988,1.);
#1804=VECTOR('',#5989,1.);
#1805=VECTOR('',#5992,1.);
#1806=VECTOR('',#5993,1.);
#1807=VECTOR('',#5994,1.);
#1808=VECTOR('',#5997,1.);
#1809=VECTOR('',#5998,1.);
#1810=VECTOR('',#6009,0.25);
#1811=VECTOR('',#6016,0.274999999999999);
#1812=VECTOR('',#6023,0.275);
#1813=VECTOR('',#6030,0.275);
#1814=VECTOR('',#6037,0.274999999999999);
#1815=VECTOR('',#6042,1.);
#1816=VECTOR('',#6043,1.);
#1817=VECTOR('',#6044,1.);
#1818=VECTOR('',#6045,1.);
#1819=VECTOR('',#6048,1.);
#1820=VECTOR('',#6049,1.);
#1821=VECTOR('',#6050,1.);
#1822=VECTOR('',#6053,1.);
#1823=VECTOR('',#6054,1.);
#1824=VECTOR('',#6055,1.);
#1825=VECTOR('',#6058,1.);
#1826=VECTOR('',#6059,1.);
#1827=VECTOR('',#6070,0.33);
#1828=VECTOR('',#6077,1.5);
#1829=VECTOR('',#6092,1.);
#1830=VECTOR('',#6093,1.);
#1831=VECTOR('',#6094,1.);
#1832=VECTOR('',#6097,1.);
#1833=VECTOR('',#6098,1.);
#1834=VECTOR('',#6099,1.);
#1835=VECTOR('',#6104,1.);
#1836=VECTOR('',#6105,1.);
#1837=VECTOR('',#6108,1.);
#1838=VECTOR('',#6109,1.);
#1839=VECTOR('',#6122,1.05);
#1840=VECTOR('',#6131,1.);
#1841=VECTOR('',#6140,1.05);
#1842=VECTOR('',#6149,1.);
#1843=VECTOR('',#6158,1.05);
#1844=VECTOR('',#6165,0.9);
#1845=VECTOR('',#6172,1.);
#1846=VECTOR('',#6175,1.);
#1847=VECTOR('',#6178,1.);
#1848=VECTOR('',#6179,1.);
#1849=VECTOR('',#6180,1.);
#1850=VECTOR('',#6187,1.);
#1851=VECTOR('',#6190,1.);
#1852=VECTOR('',#6191,1.);
#1853=VECTOR('',#6202,0.895);
#1854=VECTOR('',#6209,0.605);
#1855=VECTOR('',#6224,0.325);
#1856=VECTOR('',#6229,0.35);
#1857=VECTOR('',#6234,0.335);
#1858=VECTOR('',#6243,0.21);
#1859=VECTOR('',#6248,0.2);
#1860=VECTOR('',#6253,0.18);
#1861=VECTOR('',#6258,1.);
#1862=VECTOR('',#6259,1.);
#1863=VECTOR('',#6260,1.);
#1864=VECTOR('',#6261,1.);
#1865=VECTOR('',#6264,1.);
#1866=VECTOR('',#6265,1.);
#1867=VECTOR('',#6266,1.);
#1868=VECTOR('',#6269,1.);
#1869=VECTOR('',#6270,1.);
#1870=VECTOR('',#6271,1.);
#1871=VECTOR('',#6274,1.);
#1872=VECTOR('',#6275,1.);
#1873=VECTOR('',#6276,1.);
#1874=VECTOR('',#6279,1.);
#1875=VECTOR('',#6280,1.);
#1876=VECTOR('',#6281,1.);
#1877=VECTOR('',#6284,1.);
#1878=VECTOR('',#6285,1.);
#1879=VECTOR('',#6300,0.4);
#1880=VECTOR('',#6305,0.425);
#1881=VECTOR('',#6310,0.41);
#1882=VECTOR('',#6319,0.26);
#1883=VECTOR('',#6324,0.25);
#1884=VECTOR('',#6329,0.225);
#1885=VECTOR('',#6334,1.);
#1886=VECTOR('',#6335,1.);
#1887=VECTOR('',#6336,1.);
#1888=VECTOR('',#6337,1.);
#1889=VECTOR('',#6340,1.);
#1890=VECTOR('',#6341,1.);
#1891=VECTOR('',#6342,1.);
#1892=VECTOR('',#6345,1.);
#1893=VECTOR('',#6346,1.);
#1894=VECTOR('',#6347,1.);
#1895=VECTOR('',#6350,1.);
#1896=VECTOR('',#6351,1.);
#1897=VECTOR('',#6352,1.);
#1898=VECTOR('',#6355,1.);
#1899=VECTOR('',#6356,1.);
#1900=VECTOR('',#6357,1.);
#1901=VECTOR('',#6360,1.);
#1902=VECTOR('',#6361,1.);
#1903=VECTOR('',#6426,0.32);
#1904=VECTOR('',#6433,0.6);
#1905=VECTOR('',#6450,0.475);
#1906=VECTOR('',#6455,0.5);
#1907=VECTOR('',#6460,0.485);
#1908=VECTOR('',#6469,0.31);
#1909=VECTOR('',#6474,0.3);
#1910=VECTOR('',#6479,0.27);
#1911=VECTOR('',#6484,1.);
#1912=VECTOR('',#6485,1.);
#1913=VECTOR('',#6486,1.);
#1914=VECTOR('',#6487,1.);
#1915=VECTOR('',#6490,1.);
#1916=VECTOR('',#6491,1.);
#1917=VECTOR('',#6492,1.);
#1918=VECTOR('',#6495,1.);
#1919=VECTOR('',#6496,1.);
#1920=VECTOR('',#6497,1.);
#1921=VECTOR('',#6500,1.);
#1922=VECTOR('',#6501,1.);
#1923=VECTOR('',#6502,1.);
#1924=VECTOR('',#6505,1.);
#1925=VECTOR('',#6506,1.);
#1926=VECTOR('',#6507,1.);
#1927=VECTOR('',#6510,1.);
#1928=VECTOR('',#6511,1.);
#1929=CIRCLE('',#4653,0.210000000000001);
#1930=CIRCLE('',#4654,0.210000000000001);
#1931=CIRCLE('',#4656,0.21);
#1932=CIRCLE('',#4657,0.21);
#1933=CIRCLE('',#4659,0.21);
#1934=CIRCLE('',#4660,0.21);
#1935=CIRCLE('',#4662,0.210000000000001);
#1936=CIRCLE('',#4663,0.210000000000001);
#1937=CIRCLE('',#4665,0.210000000000001);
#1938=CIRCLE('',#4666,0.210000000000001);
#1939=CIRCLE('',#4668,0.210000000000001);
#1940=CIRCLE('',#4669,0.210000000000001);
#1941=CIRCLE('',#4671,0.21);
#1942=CIRCLE('',#4672,0.21);
#1943=CIRCLE('',#4674,0.21);
#1944=CIRCLE('',#4675,0.21);
#1945=CIRCLE('',#4677,0.21);
#1946=CIRCLE('',#4678,0.21);
#1947=CIRCLE('',#4680,0.21);
#1948=CIRCLE('',#4681,0.21);
#1949=CIRCLE('',#4683,0.210000000000001);
#1950=CIRCLE('',#4684,0.210000000000001);
#1951=CIRCLE('',#4686,0.210000000000001);
#1952=CIRCLE('',#4687,0.210000000000001);
#1953=CIRCLE('',#4696,0.475);
#1954=CIRCLE('',#4697,0.475);
#1955=CIRCLE('',#4699,0.275);
#1956=CIRCLE('',#4701,0.475);
#1957=CIRCLE('',#4702,0.475);
#1958=CIRCLE('',#4704,0.275);
#1959=CIRCLE('',#4706,0.275);
#1960=CIRCLE('',#4708,0.275);
#1961=CIRCLE('',#4724,0.475000000000001);
#1962=CIRCLE('',#4725,0.475000000000001);
#1963=CIRCLE('',#4727,0.274999999999999);
#1964=CIRCLE('',#4729,0.475000000000001);
#1965=CIRCLE('',#4730,0.475000000000001);
#1966=CIRCLE('',#4732,0.274999999999999);
#1967=CIRCLE('',#4734,0.274999999999999);
#1968=CIRCLE('',#4736,0.274999999999999);
#1969=CIRCLE('',#4752,0.6);
#1970=CIRCLE('',#4753,0.5);
#1971=CIRCLE('',#4755,0.6);
#1972=CIRCLE('',#4758,0.5);
#1973=CIRCLE('',#4762,0.525);
#1974=CIRCLE('',#4764,0.525);
#1975=CIRCLE('',#4766,0.525);
#1976=CIRCLE('',#4767,0.525);
#1977=CIRCLE('',#4770,0.275);
#1978=CIRCLE('',#4772,0.165);
#1979=CIRCLE('',#4774,0.275);
#1980=CIRCLE('',#4776,0.225);
#1981=CIRCLE('',#4777,0.225);
#1982=CIRCLE('',#4779,0.165);
#1983=CIRCLE('',#4781,0.275);
#1984=CIRCLE('',#4783,0.275);
#1985=CIRCLE('',#4785,0.6);
#1986=CIRCLE('',#4786,0.6);
#1987=CIRCLE('',#4808,0.24505);
#1988=CIRCLE('',#4810,0.375);
#1989=CIRCLE('',#4812,0.425);
#1990=CIRCLE('',#4814,0.425);
#1991=CIRCLE('',#4816,0.395);
#1992=CIRCLE('',#4818,0.27);
#1993=CIRCLE('',#4820,0.24505);
#1994=CIRCLE('',#4825,0.165);
#1995=CIRCLE('',#4826,0.165);
#1996=CIRCLE('',#4829,0.165);
#1997=CIRCLE('',#4830,0.165);
#1998=CIRCLE('',#4833,0.165);
#1999=CIRCLE('',#4834,0.165);
#2000=CIRCLE('',#4837,0.165);
#2001=CIRCLE('',#4838,0.165);
#2002=CIRCLE('',#4841,0.165);
#2003=CIRCLE('',#4842,0.165);
#2004=CIRCLE('',#4845,0.165);
#2005=CIRCLE('',#4846,0.165);
#2006=CIRCLE('',#4849,0.165);
#2007=CIRCLE('',#4850,0.165);
#2008=CIRCLE('',#4853,0.165);
#2009=CIRCLE('',#4854,0.165);
#2010=CIRCLE('',#4857,0.210000000000001);
#2011=CIRCLE('',#4858,0.210000000000001);
#2012=CIRCLE('',#4861,0.210000000000001);
#2013=CIRCLE('',#4862,0.210000000000001);
#2014=CIRCLE('',#4865,0.210000000000001);
#2015=CIRCLE('',#4866,0.210000000000001);
#2016=CIRCLE('',#4869,0.210000000000001);
#2017=CIRCLE('',#4870,0.210000000000001);
#2018=CIRCLE('',#4873,1.05);
#2019=CIRCLE('',#4874,1.05);
#2020=CIRCLE('',#4876,1.05);
#2021=CIRCLE('',#4877,1.05);
#2022=CIRCLE('',#4886,0.7);
#2023=CIRCLE('',#4887,0.7);
#2024=CIRCLE('',#4889,1.04);
#2025=CIRCLE('',#4890,1.04);
#2026=CIRCLE('',#4895,0.7);
#2027=CIRCLE('',#4896,0.7);
#2028=CIRCLE('',#4898,1.04);
#2029=CIRCLE('',#4899,1.04);
#2030=CIRCLE('',#4904,0.225);
#2031=CIRCLE('',#4905,0.225);
#2032=CIRCLE('',#4907,0.225);
#2033=CIRCLE('',#4908,0.225);
#2034=CIRCLE('',#4910,0.225);
#2035=CIRCLE('',#4911,0.225);
#2036=CIRCLE('',#4913,0.225);
#2037=CIRCLE('',#4914,0.225);
#2038=CIRCLE('',#4916,0.7);
#2039=CIRCLE('',#4917,0.7);
#2040=CIRCLE('',#4919,0.7);
#2041=CIRCLE('',#4920,0.7);
#2042=CIRCLE('',#4929,0.225);
#2043=CIRCLE('',#4930,0.225);
#2044=CIRCLE('',#4932,0.225);
#2045=CIRCLE('',#4933,0.225);
#2046=CIRCLE('',#4935,0.225);
#2047=CIRCLE('',#4936,0.225);
#2048=CIRCLE('',#4938,0.225);
#2049=CIRCLE('',#4939,0.225);
#2050=CIRCLE('',#4941,0.7);
#2051=CIRCLE('',#4942,0.7);
#2052=CIRCLE('',#4944,0.7);
#2053=CIRCLE('',#4945,0.7);
#2054=CIRCLE('',#4954,0.25);
#2055=CIRCLE('',#4955,0.25);
#2056=CIRCLE('',#4957,0.274999999999999);
#2057=CIRCLE('',#4958,0.274999999999999);
#2058=CIRCLE('',#4960,0.275);
#2059=CIRCLE('',#4961,0.275);
#2060=CIRCLE('',#4963,0.275);
#2061=CIRCLE('',#4964,0.275);
#2062=CIRCLE('',#4966,0.274999999999999);
#2063=CIRCLE('',#4967,0.274999999999999);
#2064=CIRCLE('',#4976,0.33);
#2065=CIRCLE('',#4977,0.33);
#2066=CIRCLE('',#4979,1.5);
#2067=CIRCLE('',#4980,1.5);
#2068=CIRCLE('',#4986,0.9);
#2069=CIRCLE('',#4989,0.9);
#2070=CIRCLE('',#4993,1.05);
#2071=CIRCLE('',#4994,0.9);
#2072=CIRCLE('',#4996,1.05);
#2073=CIRCLE('',#4998,1.);
#2074=CIRCLE('',#5000,1.);
#2075=CIRCLE('',#5002,1.05);
#2076=CIRCLE('',#5004,1.05);
#2077=CIRCLE('',#5006,1.);
#2078=CIRCLE('',#5008,1.);
#2079=CIRCLE('',#5010,1.05);
#2080=CIRCLE('',#5012,1.05);
#2081=CIRCLE('',#5014,0.9);
#2082=CIRCLE('',#5018,0.895);
#2083=CIRCLE('',#5019,0.605);
#2084=CIRCLE('',#5022,0.895);
#2085=CIRCLE('',#5023,0.605);
#2086=CIRCLE('',#5026,0.895);
#2087=CIRCLE('',#5027,0.605);
#2088=CIRCLE('',#5029,0.895);
#2089=CIRCLE('',#5031,0.605);
#2090=CIRCLE('',#5037,0.3);
#2091=CIRCLE('',#5039,0.35);
#2092=CIRCLE('',#5041,0.35);
#2093=CIRCLE('',#5043,0.32);
#2094=CIRCLE('',#5045,0.22);
#2095=CIRCLE('',#5047,0.1954);
#2096=CIRCLE('',#5049,0.1954);
#2097=CIRCLE('',#5051,0.16);
#2098=CIRCLE('',#5063,0.375);
#2099=CIRCLE('',#5065,0.425);
#2100=CIRCLE('',#5067,0.425);
#2101=CIRCLE('',#5069,0.395);
#2102=CIRCLE('',#5071,0.27);
#2103=CIRCLE('',#5073,0.24505);
#2104=CIRCLE('',#5075,0.24505);
#2105=CIRCLE('',#5077,0.2);
#2106=CIRCLE('',#5116,0.32);
#2107=CIRCLE('',#5117,0.32);
#2108=CIRCLE('',#5119,0.6);
#2109=CIRCLE('',#5120,0.6);
#2110=CIRCLE('',#5125,0.45);
#2111=CIRCLE('',#5127,0.5);
#2112=CIRCLE('',#5129,0.5);
#2113=CIRCLE('',#5131,0.47);
#2114=CIRCLE('',#5133,0.32);
#2115=CIRCLE('',#5135,0.2942);
#2116=CIRCLE('',#5137,0.2942);
#2117=CIRCLE('',#5139,0.24);
#2118=VERTEX_POINT('',#6574);
#2119=VERTEX_POINT('',#6576);
#2120=VERTEX_POINT('',#6580);
#2121=VERTEX_POINT('',#6582);
#2122=VERTEX_POINT('',#6586);
#2123=VERTEX_POINT('',#6588);
#2124=VERTEX_POINT('',#6592);
#2125=VERTEX_POINT('',#6594);
#2126=VERTEX_POINT('',#6598);
#2127=VERTEX_POINT('',#6600);
#2128=VERTEX_POINT('',#6604);
#2129=VERTEX_POINT('',#6606);
#2130=VERTEX_POINT('',#6610);
#2131=VERTEX_POINT('',#6612);
#2132=VERTEX_POINT('',#6616);
#2133=VERTEX_POINT('',#6618);
#2134=VERTEX_POINT('',#6622);
#2135=VERTEX_POINT('',#6624);
#2136=VERTEX_POINT('',#6628);
#2137=VERTEX_POINT('',#6630);
#2138=VERTEX_POINT('',#6634);
#2139=VERTEX_POINT('',#6636);
#2140=VERTEX_POINT('',#6640);
#2141=VERTEX_POINT('',#6642);
#2142=VERTEX_POINT('',#6646);
#2143=VERTEX_POINT('',#6647);
#2144=VERTEX_POINT('',#6649);
#2145=VERTEX_POINT('',#6651);
#2146=VERTEX_POINT('',#6655);
#2147=VERTEX_POINT('',#6657);
#2148=VERTEX_POINT('',#6661);
#2149=VERTEX_POINT('',#6663);
#2150=VERTEX_POINT('',#6673);
#2151=VERTEX_POINT('',#6675);
#2152=VERTEX_POINT('',#6679);
#2153=VERTEX_POINT('',#6682);
#2154=VERTEX_POINT('',#6684);
#2155=VERTEX_POINT('',#6688);
#2156=VERTEX_POINT('',#6691);
#2157=VERTEX_POINT('',#6695);
#2158=VERTEX_POINT('',#6699);
#2159=VERTEX_POINT('',#6700);
#2160=VERTEX_POINT('',#6702);
#2161=VERTEX_POINT('',#6704);
#2162=VERTEX_POINT('',#6708);
#2163=VERTEX_POINT('',#6710);
#2164=VERTEX_POINT('',#6714);
#2165=VERTEX_POINT('',#6716);
#2166=VERTEX_POINT('',#6726);
#2167=VERTEX_POINT('',#6727);
#2168=VERTEX_POINT('',#6729);
#2169=VERTEX_POINT('',#6731);
#2170=VERTEX_POINT('',#6735);
#2171=VERTEX_POINT('',#6737);
#2172=VERTEX_POINT('',#6741);
#2173=VERTEX_POINT('',#6743);
#2174=VERTEX_POINT('',#6753);
#2175=VERTEX_POINT('',#6755);
#2176=VERTEX_POINT('',#6759);
#2177=VERTEX_POINT('',#6762);
#2178=VERTEX_POINT('',#6764);
#2179=VERTEX_POINT('',#6768);
#2180=VERTEX_POINT('',#6771);
#2181=VERTEX_POINT('',#6775);
#2182=VERTEX_POINT('',#6779);
#2183=VERTEX_POINT('',#6780);
#2184=VERTEX_POINT('',#6782);
#2185=VERTEX_POINT('',#6784);
#2186=VERTEX_POINT('',#6788);
#2187=VERTEX_POINT('',#6790);
#2188=VERTEX_POINT('',#6794);
#2189=VERTEX_POINT('',#6796);
#2190=VERTEX_POINT('',#6806);
#2191=VERTEX_POINT('',#6807);
#2192=VERTEX_POINT('',#6809);
#2193=VERTEX_POINT('',#6811);
#2194=VERTEX_POINT('',#6815);
#2195=VERTEX_POINT('',#6817);
#2196=VERTEX_POINT('',#6821);
#2197=VERTEX_POINT('',#6823);
#2198=VERTEX_POINT('',#6833);
#2199=VERTEX_POINT('',#6835);
#2200=VERTEX_POINT('',#6839);
#2201=VERTEX_POINT('',#6844);
#2202=VERTEX_POINT('',#6850);
#2203=VERTEX_POINT('',#6851);
#2204=VERTEX_POINT('',#6855);
#2205=VERTEX_POINT('',#6857);
#2206=VERTEX_POINT('',#6861);
#2207=VERTEX_POINT('',#6862);
#2208=VERTEX_POINT('',#6864);
#2209=VERTEX_POINT('',#6866);
#2210=VERTEX_POINT('',#6872);
#2211=VERTEX_POINT('',#6874);
#2212=VERTEX_POINT('',#6876);
#2213=VERTEX_POINT('',#6878);
#2214=VERTEX_POINT('',#6881);
#2215=VERTEX_POINT('',#6884);
#2216=VERTEX_POINT('',#6886);
#2217=VERTEX_POINT('',#6889);
#2218=VERTEX_POINT('',#6892);
#2219=VERTEX_POINT('',#6893);
#2220=VERTEX_POINT('',#6895);
#2221=VERTEX_POINT('',#6898);
#2222=VERTEX_POINT('',#6901);
#2223=VERTEX_POINT('',#6904);
#2224=VERTEX_POINT('',#6906);
#2225=VERTEX_POINT('',#6910);
#2226=VERTEX_POINT('',#6914);
#2227=VERTEX_POINT('',#6918);
#2228=VERTEX_POINT('',#6922);
#2229=VERTEX_POINT('',#6924);
#2230=VERTEX_POINT('',#6928);
#2231=VERTEX_POINT('',#6930);
#2232=VERTEX_POINT('',#6933);
#2233=VERTEX_POINT('',#6935);
#2234=VERTEX_POINT('',#6937);
#2235=VERTEX_POINT('',#6939);
#2236=VERTEX_POINT('',#6941);
#2237=VERTEX_POINT('',#6945);
#2238=VERTEX_POINT('',#6949);
#2239=VERTEX_POINT('',#6955);
#2240=VERTEX_POINT('',#6959);
#2241=VERTEX_POINT('',#6963);
#2242=VERTEX_POINT('',#6967);
#2243=VERTEX_POINT('',#6971);
#2244=VERTEX_POINT('',#6979);
#2245=VERTEX_POINT('',#6980);
#2246=VERTEX_POINT('',#6982);
#2247=VERTEX_POINT('',#6984);
#2248=VERTEX_POINT('',#6988);
#2249=VERTEX_POINT('',#6990);
#2250=VERTEX_POINT('',#6994);
#2251=VERTEX_POINT('',#6996);
#2252=VERTEX_POINT('',#7000);
#2253=VERTEX_POINT('',#7002);
#2254=VERTEX_POINT('',#7006);
#2255=VERTEX_POINT('',#7008);
#2256=VERTEX_POINT('',#7017);
#2257=VERTEX_POINT('',#7020);
#2258=VERTEX_POINT('',#7023);
#2259=VERTEX_POINT('',#7027);
#2260=VERTEX_POINT('',#7031);
#2261=VERTEX_POINT('',#7035);
#2262=VERTEX_POINT('',#7038);
#2263=VERTEX_POINT('',#7046);
#2264=VERTEX_POINT('',#7048);
#2265=VERTEX_POINT('',#7053);
#2266=VERTEX_POINT('',#7055);
#2267=VERTEX_POINT('',#7060);
#2268=VERTEX_POINT('',#7062);
#2269=VERTEX_POINT('',#7067);
#2270=VERTEX_POINT('',#7069);
#2271=VERTEX_POINT('',#7074);
#2272=VERTEX_POINT('',#7076);
#2273=VERTEX_POINT('',#7081);
#2274=VERTEX_POINT('',#7083);
#2275=VERTEX_POINT('',#7088);
#2276=VERTEX_POINT('',#7090);
#2277=VERTEX_POINT('',#7095);
#2278=VERTEX_POINT('',#7097);
#2279=VERTEX_POINT('',#7102);
#2280=VERTEX_POINT('',#7104);
#2281=VERTEX_POINT('',#7109);
#2282=VERTEX_POINT('',#7111);
#2283=VERTEX_POINT('',#7116);
#2284=VERTEX_POINT('',#7118);
#2285=VERTEX_POINT('',#7123);
#2286=VERTEX_POINT('',#7125);
#2287=VERTEX_POINT('',#7130);
#2288=VERTEX_POINT('',#7132);
#2289=VERTEX_POINT('',#7136);
#2290=VERTEX_POINT('',#7138);
#2291=VERTEX_POINT('',#7142);
#2292=VERTEX_POINT('',#7143);
#2293=VERTEX_POINT('',#7145);
#2294=VERTEX_POINT('',#7147);
#2295=VERTEX_POINT('',#7151);
#2296=VERTEX_POINT('',#7153);
#2297=VERTEX_POINT('',#7157);
#2298=VERTEX_POINT('',#7159);
#2299=VERTEX_POINT('',#7169);
#2300=VERTEX_POINT('',#7171);
#2301=VERTEX_POINT('',#7175);
#2302=VERTEX_POINT('',#7177);
#2303=VERTEX_POINT('',#7184);
#2304=VERTEX_POINT('',#7186);
#2305=VERTEX_POINT('',#7190);
#2306=VERTEX_POINT('',#7192);
#2307=VERTEX_POINT('',#7199);
#2308=VERTEX_POINT('',#7201);
#2309=VERTEX_POINT('',#7205);
#2310=VERTEX_POINT('',#7207);
#2311=VERTEX_POINT('',#7211);
#2312=VERTEX_POINT('',#7213);
#2313=VERTEX_POINT('',#7217);
#2314=VERTEX_POINT('',#7219);
#2315=VERTEX_POINT('',#7223);
#2316=VERTEX_POINT('',#7225);
#2317=VERTEX_POINT('',#7229);
#2318=VERTEX_POINT('',#7231);
#2319=VERTEX_POINT('',#7235);
#2320=VERTEX_POINT('',#7236);
#2321=VERTEX_POINT('',#7238);
#2322=VERTEX_POINT('',#7240);
#2323=VERTEX_POINT('',#7244);
#2324=VERTEX_POINT('',#7246);
#2325=VERTEX_POINT('',#7250);
#2326=VERTEX_POINT('',#7252);
#2327=VERTEX_POINT('',#7262);
#2328=VERTEX_POINT('',#7264);
#2329=VERTEX_POINT('',#7268);
#2330=VERTEX_POINT('',#7270);
#2331=VERTEX_POINT('',#7274);
#2332=VERTEX_POINT('',#7276);
#2333=VERTEX_POINT('',#7280);
#2334=VERTEX_POINT('',#7282);
#2335=VERTEX_POINT('',#7286);
#2336=VERTEX_POINT('',#7288);
#2337=VERTEX_POINT('',#7292);
#2338=VERTEX_POINT('',#7294);
#2339=VERTEX_POINT('',#7298);
#2340=VERTEX_POINT('',#7299);
#2341=VERTEX_POINT('',#7301);
#2342=VERTEX_POINT('',#7303);
#2343=VERTEX_POINT('',#7307);
#2344=VERTEX_POINT('',#7309);
#2345=VERTEX_POINT('',#7313);
#2346=VERTEX_POINT('',#7315);
#2347=VERTEX_POINT('',#7325);
#2348=VERTEX_POINT('',#7327);
#2349=VERTEX_POINT('',#7331);
#2350=VERTEX_POINT('',#7333);
#2351=VERTEX_POINT('',#7337);
#2352=VERTEX_POINT('',#7339);
#2353=VERTEX_POINT('',#7343);
#2354=VERTEX_POINT('',#7345);
#2355=VERTEX_POINT('',#7349);
#2356=VERTEX_POINT('',#7351);
#2357=VERTEX_POINT('',#7355);
#2358=VERTEX_POINT('',#7356);
#2359=VERTEX_POINT('',#7358);
#2360=VERTEX_POINT('',#7360);
#2361=VERTEX_POINT('',#7364);
#2362=VERTEX_POINT('',#7366);
#2363=VERTEX_POINT('',#7370);
#2364=VERTEX_POINT('',#7372);
#2365=VERTEX_POINT('',#7382);
#2366=VERTEX_POINT('',#7384);
#2367=VERTEX_POINT('',#7388);
#2368=VERTEX_POINT('',#7390);
#2369=VERTEX_POINT('',#7398);
#2370=VERTEX_POINT('',#7399);
#2371=VERTEX_POINT('',#7401);
#2372=VERTEX_POINT('',#7403);
#2373=VERTEX_POINT('',#7407);
#2374=VERTEX_POINT('',#7409);
#2375=VERTEX_POINT('',#7413);
#2376=VERTEX_POINT('',#7415);
#2377=VERTEX_POINT('',#7423);
#2378=VERTEX_POINT('',#7425);
#2379=VERTEX_POINT('',#7428);
#2380=VERTEX_POINT('',#7432);
#2381=VERTEX_POINT('',#7435);
#2382=VERTEX_POINT('',#7439);
#2383=VERTEX_POINT('',#7442);
#2384=VERTEX_POINT('',#7446);
#2385=VERTEX_POINT('',#7449);
#2386=VERTEX_POINT('',#7453);
#2387=VERTEX_POINT('',#7456);
#2388=VERTEX_POINT('',#7460);
#2389=VERTEX_POINT('',#7466);
#2390=VERTEX_POINT('',#7467);
#2391=VERTEX_POINT('',#7469);
#2392=VERTEX_POINT('',#7471);
#2393=VERTEX_POINT('',#7475);
#2394=VERTEX_POINT('',#7477);
#2395=VERTEX_POINT('',#7481);
#2396=VERTEX_POINT('',#7483);
#2397=VERTEX_POINT('',#7490);
#2398=VERTEX_POINT('',#7492);
#2399=VERTEX_POINT('',#7495);
#2400=VERTEX_POINT('',#7499);
#2401=VERTEX_POINT('',#7507);
#2402=VERTEX_POINT('',#7510);
#2403=VERTEX_POINT('',#7514);
#2404=VERTEX_POINT('',#7518);
#2405=VERTEX_POINT('',#7522);
#2406=VERTEX_POINT('',#7525);
#2407=VERTEX_POINT('',#7529);
#2408=VERTEX_POINT('',#7533);
#2409=VERTEX_POINT('',#7538);
#2410=VERTEX_POINT('',#7539);
#2411=VERTEX_POINT('',#7541);
#2412=VERTEX_POINT('',#7543);
#2413=VERTEX_POINT('',#7547);
#2414=VERTEX_POINT('',#7549);
#2415=VERTEX_POINT('',#7553);
#2416=VERTEX_POINT('',#7555);
#2417=VERTEX_POINT('',#7559);
#2418=VERTEX_POINT('',#7561);
#2419=VERTEX_POINT('',#7565);
#2420=VERTEX_POINT('',#7567);
#2421=VERTEX_POINT('',#7577);
#2422=VERTEX_POINT('',#7580);
#2423=VERTEX_POINT('',#7584);
#2424=VERTEX_POINT('',#7588);
#2425=VERTEX_POINT('',#7592);
#2426=VERTEX_POINT('',#7595);
#2427=VERTEX_POINT('',#7599);
#2428=VERTEX_POINT('',#7603);
#2429=VERTEX_POINT('',#7608);
#2430=VERTEX_POINT('',#7609);
#2431=VERTEX_POINT('',#7611);
#2432=VERTEX_POINT('',#7613);
#2433=VERTEX_POINT('',#7617);
#2434=VERTEX_POINT('',#7619);
#2435=VERTEX_POINT('',#7623);
#2436=VERTEX_POINT('',#7625);
#2437=VERTEX_POINT('',#7629);
#2438=VERTEX_POINT('',#7631);
#2439=VERTEX_POINT('',#7635);
#2440=VERTEX_POINT('',#7637);
#2441=VERTEX_POINT('',#7674);
#2442=VERTEX_POINT('',#7676);
#2443=VERTEX_POINT('',#7680);
#2444=VERTEX_POINT('',#7682);
#2445=VERTEX_POINT('',#7689);
#2446=VERTEX_POINT('',#7692);
#2447=VERTEX_POINT('',#7696);
#2448=VERTEX_POINT('',#7700);
#2449=VERTEX_POINT('',#7704);
#2450=VERTEX_POINT('',#7707);
#2451=VERTEX_POINT('',#7711);
#2452=VERTEX_POINT('',#7715);
#2453=VERTEX_POINT('',#7720);
#2454=VERTEX_POINT('',#7721);
#2455=VERTEX_POINT('',#7723);
#2456=VERTEX_POINT('',#7725);
#2457=VERTEX_POINT('',#7729);
#2458=VERTEX_POINT('',#7731);
#2459=VERTEX_POINT('',#7735);
#2460=VERTEX_POINT('',#7737);
#2461=VERTEX_POINT('',#7741);
#2462=VERTEX_POINT('',#7743);
#2463=VERTEX_POINT('',#7747);
#2464=VERTEX_POINT('',#7749);
#2465=EDGE_CURVE('',#2118,#2118,#1929,.T.);
#2466=EDGE_CURVE('',#2118,#2119,#1249,.T.);
#2467=EDGE_CURVE('',#2119,#2119,#1930,.T.);
#2468=EDGE_CURVE('',#2120,#2120,#1931,.T.);
#2469=EDGE_CURVE('',#2120,#2121,#1250,.T.);
#2470=EDGE_CURVE('',#2121,#2121,#1932,.T.);
#2471=EDGE_CURVE('',#2122,#2122,#1933,.T.);
#2472=EDGE_CURVE('',#2122,#2123,#1251,.T.);
#2473=EDGE_CURVE('',#2123,#2123,#1934,.T.);
#2474=EDGE_CURVE('',#2124,#2124,#1935,.T.);
#2475=EDGE_CURVE('',#2124,#2125,#1252,.T.);
#2476=EDGE_CURVE('',#2125,#2125,#1936,.T.);
#2477=EDGE_CURVE('',#2126,#2126,#1937,.T.);
#2478=EDGE_CURVE('',#2126,#2127,#1253,.T.);
#2479=EDGE_CURVE('',#2127,#2127,#1938,.T.);
#2480=EDGE_CURVE('',#2128,#2128,#1939,.T.);
#2481=EDGE_CURVE('',#2128,#2129,#1254,.T.);
#2482=EDGE_CURVE('',#2129,#2129,#1940,.T.);
#2483=EDGE_CURVE('',#2130,#2130,#1941,.T.);
#2484=EDGE_CURVE('',#2130,#2131,#1255,.T.);
#2485=EDGE_CURVE('',#2131,#2131,#1942,.T.);
#2486=EDGE_CURVE('',#2132,#2132,#1943,.T.);
#2487=EDGE_CURVE('',#2132,#2133,#1256,.T.);
#2488=EDGE_CURVE('',#2133,#2133,#1944,.T.);
#2489=EDGE_CURVE('',#2134,#2134,#1945,.T.);
#2490=EDGE_CURVE('',#2134,#2135,#1257,.T.);
#2491=EDGE_CURVE('',#2135,#2135,#1946,.T.);
#2492=EDGE_CURVE('',#2136,#2136,#1947,.T.);
#2493=EDGE_CURVE('',#2136,#2137,#1258,.T.);
#2494=EDGE_CURVE('',#2137,#2137,#1948,.T.);
#2495=EDGE_CURVE('',#2138,#2138,#1949,.T.);
#2496=EDGE_CURVE('',#2138,#2139,#1259,.T.);
#2497=EDGE_CURVE('',#2139,#2139,#1950,.T.);
#2498=EDGE_CURVE('',#2140,#2140,#1951,.T.);
#2499=EDGE_CURVE('',#2140,#2141,#1260,.T.);
#2500=EDGE_CURVE('',#2141,#2141,#1952,.T.);
#2501=EDGE_CURVE('',#2142,#2143,#1261,.T.);
#2502=EDGE_CURVE('',#2143,#2144,#1262,.T.);
#2503=EDGE_CURVE('',#2145,#2144,#1263,.T.);
#2504=EDGE_CURVE('',#2142,#2145,#1264,.T.);
#2505=EDGE_CURVE('',#2146,#2142,#1265,.T.);
#2506=EDGE_CURVE('',#2147,#2145,#1266,.T.);
#2507=EDGE_CURVE('',#2146,#2147,#1267,.T.);
#2508=EDGE_CURVE('',#2148,#2146,#1268,.T.);
#2509=EDGE_CURVE('',#2149,#2147,#1269,.T.);
#2510=EDGE_CURVE('',#2148,#2149,#1270,.T.);
#2511=EDGE_CURVE('',#2143,#2148,#1271,.T.);
#2512=EDGE_CURVE('',#2144,#2149,#1272,.T.);
#2513=EDGE_CURVE('',#2150,#2150,#1953,.T.);
#2514=EDGE_CURVE('',#2150,#2151,#1273,.T.);
#2515=EDGE_CURVE('',#2151,#2151,#1954,.T.);
#2516=EDGE_CURVE('',#2152,#2152,#1955,.T.);
#2517=EDGE_CURVE('',#2153,#2153,#1956,.T.);
#2518=EDGE_CURVE('',#2153,#2154,#1274,.T.);
#2519=EDGE_CURVE('',#2154,#2154,#1957,.T.);
#2520=EDGE_CURVE('',#2155,#2155,#1958,.T.);
#2521=EDGE_CURVE('',#2156,#2156,#1959,.T.);
#2522=EDGE_CURVE('',#2156,#2152,#1275,.T.);
#2523=EDGE_CURVE('',#2157,#2157,#1960,.T.);
#2524=EDGE_CURVE('',#2157,#2155,#1276,.T.);
#2525=EDGE_CURVE('',#2158,#2159,#1277,.T.);
#2526=EDGE_CURVE('',#2159,#2160,#1278,.T.);
#2527=EDGE_CURVE('',#2161,#2160,#1279,.T.);
#2528=EDGE_CURVE('',#2158,#2161,#1280,.T.);
#2529=EDGE_CURVE('',#2162,#2158,#1281,.T.);
#2530=EDGE_CURVE('',#2163,#2161,#1282,.T.);
#2531=EDGE_CURVE('',#2162,#2163,#1283,.T.);
#2532=EDGE_CURVE('',#2164,#2162,#1284,.T.);
#2533=EDGE_CURVE('',#2165,#2163,#1285,.T.);
#2534=EDGE_CURVE('',#2164,#2165,#1286,.T.);
#2535=EDGE_CURVE('',#2159,#2164,#1287,.T.);
#2536=EDGE_CURVE('',#2160,#2165,#1288,.T.);
#2537=EDGE_CURVE('',#2166,#2167,#1289,.T.);
#2538=EDGE_CURVE('',#2167,#2168,#1290,.T.);
#2539=EDGE_CURVE('',#2169,#2168,#1291,.T.);
#2540=EDGE_CURVE('',#2166,#2169,#1292,.T.);
#2541=EDGE_CURVE('',#2170,#2166,#1293,.T.);
#2542=EDGE_CURVE('',#2171,#2169,#1294,.T.);
#2543=EDGE_CURVE('',#2170,#2171,#1295,.T.);
#2544=EDGE_CURVE('',#2172,#2170,#1296,.T.);
#2545=EDGE_CURVE('',#2173,#2171,#1297,.T.);
#2546=EDGE_CURVE('',#2172,#2173,#1298,.T.);
#2547=EDGE_CURVE('',#2167,#2172,#1299,.T.);
#2548=EDGE_CURVE('',#2168,#2173,#1300,.T.);
#2549=EDGE_CURVE('',#2174,#2174,#1961,.T.);
#2550=EDGE_CURVE('',#2174,#2175,#1301,.T.);
#2551=EDGE_CURVE('',#2175,#2175,#1962,.T.);
#2552=EDGE_CURVE('',#2176,#2176,#1963,.T.);
#2553=EDGE_CURVE('',#2177,#2177,#1964,.T.);
#2554=EDGE_CURVE('',#2177,#2178,#1302,.T.);
#2555=EDGE_CURVE('',#2178,#2178,#1965,.T.);
#2556=EDGE_CURVE('',#2179,#2179,#1966,.T.);
#2557=EDGE_CURVE('',#2180,#2180,#1967,.T.);
#2558=EDGE_CURVE('',#2180,#2176,#1303,.T.);
#2559=EDGE_CURVE('',#2181,#2181,#1968,.T.);
#2560=EDGE_CURVE('',#2181,#2179,#1304,.T.);
#2561=EDGE_CURVE('',#2182,#2183,#1305,.T.);
#2562=EDGE_CURVE('',#2183,#2184,#1306,.T.);
#2563=EDGE_CURVE('',#2185,#2184,#1307,.T.);
#2564=EDGE_CURVE('',#2182,#2185,#1308,.T.);
#2565=EDGE_CURVE('',#2186,#2182,#1309,.T.);
#2566=EDGE_CURVE('',#2187,#2185,#1310,.T.);
#2567=EDGE_CURVE('',#2186,#2187,#1311,.T.);
#2568=EDGE_CURVE('',#2188,#2186,#1312,.T.);
#2569=EDGE_CURVE('',#2189,#2187,#1313,.T.);
#2570=EDGE_CURVE('',#2188,#2189,#1314,.T.);
#2571=EDGE_CURVE('',#2183,#2188,#1315,.T.);
#2572=EDGE_CURVE('',#2184,#2189,#1316,.T.);
#2573=EDGE_CURVE('',#2190,#2191,#1317,.T.);
#2574=EDGE_CURVE('',#2191,#2192,#1318,.T.);
#2575=EDGE_CURVE('',#2193,#2192,#1319,.T.);
#2576=EDGE_CURVE('',#2190,#2193,#1320,.T.);
#2577=EDGE_CURVE('',#2194,#2190,#1321,.T.);
#2578=EDGE_CURVE('',#2195,#2193,#1322,.T.);
#2579=EDGE_CURVE('',#2194,#2195,#1323,.T.);
#2580=EDGE_CURVE('',#2196,#2194,#1324,.T.);
#2581=EDGE_CURVE('',#2197,#2195,#1325,.T.);
#2582=EDGE_CURVE('',#2196,#2197,#1326,.T.);
#2583=EDGE_CURVE('',#2191,#2196,#1327,.T.);
#2584=EDGE_CURVE('',#2192,#2197,#1328,.T.);
#2585=EDGE_CURVE('',#2198,#2198,#1969,.T.);
#2586=EDGE_CURVE('',#2198,#2199,#1329,.T.);
#2587=EDGE_CURVE('',#2199,#2199,#1970,.T.);
#2588=EDGE_CURVE('',#2200,#2200,#1971,.T.);
#2589=EDGE_CURVE('',#2200,#2198,#1330,.T.);
#2590=EDGE_CURVE('',#2201,#2201,#1972,.T.);
#2591=EDGE_CURVE('',#2201,#2200,#1331,.T.);
#2592=EDGE_CURVE('',#2202,#2203,#1332,.T.);
#2593=EDGE_CURVE('',#2203,#2202,#1973,.T.);
#2594=EDGE_CURVE('',#2204,#2202,#1333,.T.);
#2595=EDGE_CURVE('',#2205,#2204,#1974,.T.);
#2596=EDGE_CURVE('',#2203,#2205,#1334,.T.);
#2597=EDGE_CURVE('',#2206,#2207,#1335,.T.);
#2598=EDGE_CURVE('',#2206,#2208,#1975,.T.);
#2599=EDGE_CURVE('',#2209,#2208,#1336,.T.);
#2600=EDGE_CURVE('',#2207,#2209,#1976,.T.);
#2601=EDGE_CURVE('',#2208,#2206,#1337,.T.);
#2602=EDGE_CURVE('',#2204,#2210,#1338,.T.);
#2603=EDGE_CURVE('',#2211,#2210,#1339,.T.);
#2604=EDGE_CURVE('',#2211,#2212,#1340,.T.);
#2605=EDGE_CURVE('',#2213,#2212,#1341,.T.);
#2606=EDGE_CURVE('',#2213,#2205,#1342,.T.);
#2607=EDGE_CURVE('',#2214,#2214,#1977,.T.);
#2608=EDGE_CURVE('',#2215,#2213,#1343,.T.);
#2609=EDGE_CURVE('',#2215,#2216,#1344,.T.);
#2610=EDGE_CURVE('',#2210,#2216,#1345,.T.);
#2611=EDGE_CURVE('',#2217,#2217,#1978,.T.);
#2612=EDGE_CURVE('',#2218,#2219,#1346,.T.);
#2613=EDGE_CURVE('',#2220,#2219,#1347,.T.);
#2614=EDGE_CURVE('',#2207,#2220,#1348,.T.);
#2615=EDGE_CURVE('',#2221,#2209,#1349,.T.);
#2616=EDGE_CURVE('',#2218,#2221,#1350,.T.);
#2617=EDGE_CURVE('',#2222,#2222,#1979,.T.);
#2618=EDGE_CURVE('',#2223,#2223,#1980,.T.);
#2619=EDGE_CURVE('',#2223,#2224,#1351,.T.);
#2620=EDGE_CURVE('',#2224,#2224,#1981,.T.);
#2621=EDGE_CURVE('',#2217,#2225,#1352,.T.);
#2622=EDGE_CURVE('',#2225,#2225,#1982,.T.);
#2623=EDGE_CURVE('',#2226,#2226,#1983,.T.);
#2624=EDGE_CURVE('',#2226,#2214,#1353,.T.);
#2625=EDGE_CURVE('',#2227,#2227,#1984,.T.);
#2626=EDGE_CURVE('',#2227,#2222,#1354,.T.);
#2627=EDGE_CURVE('',#2228,#2228,#1985,.T.);
#2628=EDGE_CURVE('',#2228,#2229,#1355,.T.);
#2629=EDGE_CURVE('',#2229,#2229,#1986,.T.);
#2630=EDGE_CURVE('',#2212,#2230,#1356,.T.);
#2631=EDGE_CURVE('',#2230,#2231,#1357,.T.);
#2632=EDGE_CURVE('',#2231,#2218,#1358,.T.);
#2633=EDGE_CURVE('',#2221,#2232,#1359,.T.);
#2634=EDGE_CURVE('',#2232,#2233,#1360,.T.);
#2635=EDGE_CURVE('',#2233,#2234,#1361,.T.);
#2636=EDGE_CURVE('',#2234,#2235,#1362,.T.);
#2637=EDGE_CURVE('',#2235,#2236,#1363,.T.);
#2638=EDGE_CURVE('',#2236,#2215,#1364,.T.);
#2639=EDGE_CURVE('',#2237,#2211,#1365,.T.);
#2640=EDGE_CURVE('',#2230,#2237,#1366,.T.);
#2641=EDGE_CURVE('',#2238,#2237,#1367,.T.);
#2642=EDGE_CURVE('',#2231,#2238,#1368,.T.);
#2643=EDGE_CURVE('',#2219,#2238,#1369,.T.);
#2644=EDGE_CURVE('',#2239,#2220,#1370,.T.);
#2645=EDGE_CURVE('',#2232,#2239,#1371,.T.);
#2646=EDGE_CURVE('',#2240,#2239,#1372,.T.);
#2647=EDGE_CURVE('',#2233,#2240,#1373,.T.);
#2648=EDGE_CURVE('',#2241,#2240,#1374,.T.);
#2649=EDGE_CURVE('',#2234,#2241,#1375,.T.);
#2650=EDGE_CURVE('',#2242,#2241,#1376,.T.);
#2651=EDGE_CURVE('',#2235,#2242,#1377,.T.);
#2652=EDGE_CURVE('',#2243,#2242,#1378,.T.);
#2653=EDGE_CURVE('',#2236,#2243,#1379,.T.);
#2654=EDGE_CURVE('',#2216,#2243,#1380,.T.);
#2655=EDGE_CURVE('',#2244,#2245,#1381,.T.);
#2656=EDGE_CURVE('',#2245,#2246,#1382,.T.);
#2657=EDGE_CURVE('',#2246,#2247,#1383,.T.);
#2658=EDGE_CURVE('',#2244,#2247,#1384,.T.);
#2659=EDGE_CURVE('',#2245,#2248,#1385,.T.);
#2660=EDGE_CURVE('',#2248,#2249,#1386,.T.);
#2661=EDGE_CURVE('',#2249,#2246,#1387,.T.);
#2662=EDGE_CURVE('',#2248,#2250,#1388,.T.);
#2663=EDGE_CURVE('',#2250,#2251,#1389,.T.);
#2664=EDGE_CURVE('',#2251,#2249,#1390,.T.);
#2665=EDGE_CURVE('',#2250,#2252,#1391,.T.);
#2666=EDGE_CURVE('',#2252,#2253,#1392,.T.);
#2667=EDGE_CURVE('',#2253,#2251,#1393,.T.);
#2668=EDGE_CURVE('',#2252,#2254,#1394,.T.);
#2669=EDGE_CURVE('',#2254,#2255,#1395,.T.);
#2670=EDGE_CURVE('',#2255,#2253,#1396,.T.);
#2671=EDGE_CURVE('',#2254,#2244,#1397,.T.);
#2672=EDGE_CURVE('',#2247,#2255,#1398,.T.);
#2673=EDGE_CURVE('',#2256,#2256,#1987,.T.);
#2674=EDGE_CURVE('',#2257,#2257,#1988,.T.);
#2675=EDGE_CURVE('',#2258,#2258,#1989,.T.);
#2676=EDGE_CURVE('',#2258,#2257,#1399,.T.);
#2677=EDGE_CURVE('',#2259,#2259,#1990,.T.);
#2678=EDGE_CURVE('',#2259,#2258,#1400,.T.);
#2679=EDGE_CURVE('',#2260,#2260,#1991,.T.);
#2680=EDGE_CURVE('',#2260,#2259,#1401,.T.);
#2681=EDGE_CURVE('',#2261,#2261,#1992,.T.);
#2682=EDGE_CURVE('',#2262,#2262,#1993,.F.);
#2683=EDGE_CURVE('',#2262,#2261,#1402,.T.);
#2684=EDGE_CURVE('',#2256,#2262,#1403,.T.);
#2685=EDGE_CURVE('',#2263,#2263,#1994,.T.);
#2686=EDGE_CURVE('',#2263,#2264,#1404,.T.);
#2687=EDGE_CURVE('',#2264,#2264,#1995,.T.);
#2688=EDGE_CURVE('',#2265,#2265,#1996,.T.);
#2689=EDGE_CURVE('',#2265,#2266,#1405,.T.);
#2690=EDGE_CURVE('',#2266,#2266,#1997,.T.);
#2691=EDGE_CURVE('',#2267,#2267,#1998,.T.);
#2692=EDGE_CURVE('',#2267,#2268,#1406,.T.);
#2693=EDGE_CURVE('',#2268,#2268,#1999,.T.);
#2694=EDGE_CURVE('',#2269,#2269,#2000,.T.);
#2695=EDGE_CURVE('',#2269,#2270,#1407,.T.);
#2696=EDGE_CURVE('',#2270,#2270,#2001,.T.);
#2697=EDGE_CURVE('',#2271,#2271,#2002,.T.);
#2698=EDGE_CURVE('',#2271,#2272,#1408,.T.);
#2699=EDGE_CURVE('',#2272,#2272,#2003,.T.);
#2700=EDGE_CURVE('',#2273,#2273,#2004,.T.);
#2701=EDGE_CURVE('',#2273,#2274,#1409,.T.);
#2702=EDGE_CURVE('',#2274,#2274,#2005,.T.);
#2703=EDGE_CURVE('',#2275,#2275,#2006,.T.);
#2704=EDGE_CURVE('',#2275,#2276,#1410,.T.);
#2705=EDGE_CURVE('',#2276,#2276,#2007,.T.);
#2706=EDGE_CURVE('',#2277,#2277,#2008,.T.);
#2707=EDGE_CURVE('',#2277,#2278,#1411,.T.);
#2708=EDGE_CURVE('',#2278,#2278,#2009,.T.);
#2709=EDGE_CURVE('',#2279,#2279,#2010,.T.);
#2710=EDGE_CURVE('',#2279,#2280,#1412,.T.);
#2711=EDGE_CURVE('',#2280,#2280,#2011,.T.);
#2712=EDGE_CURVE('',#2281,#2281,#2012,.T.);
#2713=EDGE_CURVE('',#2281,#2282,#1413,.T.);
#2714=EDGE_CURVE('',#2282,#2282,#2013,.T.);
#2715=EDGE_CURVE('',#2283,#2283,#2014,.T.);
#2716=EDGE_CURVE('',#2283,#2284,#1414,.T.);
#2717=EDGE_CURVE('',#2284,#2284,#2015,.T.);
#2718=EDGE_CURVE('',#2285,#2285,#2016,.T.);
#2719=EDGE_CURVE('',#2285,#2286,#1415,.T.);
#2720=EDGE_CURVE('',#2286,#2286,#2017,.T.);
#2721=EDGE_CURVE('',#2287,#2287,#2018,.T.);
#2722=EDGE_CURVE('',#2287,#2288,#1416,.T.);
#2723=EDGE_CURVE('',#2288,#2288,#2019,.T.);
#2724=EDGE_CURVE('',#2289,#2289,#2020,.T.);
#2725=EDGE_CURVE('',#2289,#2290,#1417,.T.);
#2726=EDGE_CURVE('',#2290,#2290,#2021,.T.);
#2727=EDGE_CURVE('',#2291,#2292,#1418,.T.);
#2728=EDGE_CURVE('',#2292,#2293,#1419,.T.);
#2729=EDGE_CURVE('',#2294,#2293,#1420,.T.);
#2730=EDGE_CURVE('',#2291,#2294,#1421,.T.);
#2731=EDGE_CURVE('',#2295,#2291,#1422,.T.);
#2732=EDGE_CURVE('',#2296,#2294,#1423,.T.);
#2733=EDGE_CURVE('',#2295,#2296,#1424,.T.);
#2734=EDGE_CURVE('',#2297,#2295,#1425,.T.);
#2735=EDGE_CURVE('',#2298,#2296,#1426,.T.);
#2736=EDGE_CURVE('',#2297,#2298,#1427,.T.);
#2737=EDGE_CURVE('',#2292,#2297,#1428,.T.);
#2738=EDGE_CURVE('',#2293,#2298,#1429,.T.);
#2739=EDGE_CURVE('',#2299,#2299,#2022,.T.);
#2740=EDGE_CURVE('',#2299,#2300,#1430,.T.);
#2741=EDGE_CURVE('',#2300,#2300,#2023,.T.);
#2742=EDGE_CURVE('',#2301,#2301,#2024,.T.);
#2743=EDGE_CURVE('',#2301,#2302,#1431,.T.);
#2744=EDGE_CURVE('',#2302,#2302,#2025,.T.);
#2745=EDGE_CURVE('',#2303,#2303,#2026,.T.);
#2746=EDGE_CURVE('',#2303,#2304,#1432,.T.);
#2747=EDGE_CURVE('',#2304,#2304,#2027,.T.);
#2748=EDGE_CURVE('',#2305,#2305,#2028,.T.);
#2749=EDGE_CURVE('',#2305,#2306,#1433,.T.);
#2750=EDGE_CURVE('',#2306,#2306,#2029,.T.);
#2751=EDGE_CURVE('',#2307,#2307,#2030,.T.);
#2752=EDGE_CURVE('',#2307,#2308,#1434,.T.);
#2753=EDGE_CURVE('',#2308,#2308,#2031,.T.);
#2754=EDGE_CURVE('',#2309,#2309,#2032,.T.);
#2755=EDGE_CURVE('',#2309,#2310,#1435,.T.);
#2756=EDGE_CURVE('',#2310,#2310,#2033,.T.);
#2757=EDGE_CURVE('',#2311,#2311,#2034,.T.);
#2758=EDGE_CURVE('',#2311,#2312,#1436,.T.);
#2759=EDGE_CURVE('',#2312,#2312,#2035,.T.);
#2760=EDGE_CURVE('',#2313,#2313,#2036,.T.);
#2761=EDGE_CURVE('',#2313,#2314,#1437,.T.);
#2762=EDGE_CURVE('',#2314,#2314,#2037,.T.);
#2763=EDGE_CURVE('',#2315,#2315,#2038,.T.);
#2764=EDGE_CURVE('',#2315,#2316,#1438,.T.);
#2765=EDGE_CURVE('',#2316,#2316,#2039,.T.);
#2766=EDGE_CURVE('',#2317,#2317,#2040,.T.);
#2767=EDGE_CURVE('',#2317,#2318,#1439,.T.);
#2768=EDGE_CURVE('',#2318,#2318,#2041,.T.);
#2769=EDGE_CURVE('',#2319,#2320,#1440,.T.);
#2770=EDGE_CURVE('',#2320,#2321,#1441,.T.);
#2771=EDGE_CURVE('',#2322,#2321,#1442,.T.);
#2772=EDGE_CURVE('',#2319,#2322,#1443,.T.);
#2773=EDGE_CURVE('',#2323,#2319,#1444,.T.);
#2774=EDGE_CURVE('',#2324,#2322,#1445,.T.);
#2775=EDGE_CURVE('',#2323,#2324,#1446,.T.);
#2776=EDGE_CURVE('',#2325,#2323,#1447,.T.);
#2777=EDGE_CURVE('',#2326,#2324,#1448,.T.);
#2778=EDGE_CURVE('',#2325,#2326,#1449,.T.);
#2779=EDGE_CURVE('',#2320,#2325,#1450,.T.);
#2780=EDGE_CURVE('',#2321,#2326,#1451,.T.);
#2781=EDGE_CURVE('',#2327,#2327,#2042,.T.);
#2782=EDGE_CURVE('',#2327,#2328,#1452,.T.);
#2783=EDGE_CURVE('',#2328,#2328,#2043,.T.);
#2784=EDGE_CURVE('',#2329,#2329,#2044,.T.);
#2785=EDGE_CURVE('',#2329,#2330,#1453,.T.);
#2786=EDGE_CURVE('',#2330,#2330,#2045,.T.);
#2787=EDGE_CURVE('',#2331,#2331,#2046,.T.);
#2788=EDGE_CURVE('',#2331,#2332,#1454,.T.);
#2789=EDGE_CURVE('',#2332,#2332,#2047,.T.);
#2790=EDGE_CURVE('',#2333,#2333,#2048,.T.);
#2791=EDGE_CURVE('',#2333,#2334,#1455,.T.);
#2792=EDGE_CURVE('',#2334,#2334,#2049,.T.);
#2793=EDGE_CURVE('',#2335,#2335,#2050,.T.);
#2794=EDGE_CURVE('',#2335,#2336,#1456,.T.);
#2795=EDGE_CURVE('',#2336,#2336,#2051,.T.);
#2796=EDGE_CURVE('',#2337,#2337,#2052,.T.);
#2797=EDGE_CURVE('',#2337,#2338,#1457,.T.);
#2798=EDGE_CURVE('',#2338,#2338,#2053,.T.);
#2799=EDGE_CURVE('',#2339,#2340,#1458,.T.);
#2800=EDGE_CURVE('',#2340,#2341,#1459,.T.);
#2801=EDGE_CURVE('',#2342,#2341,#1460,.T.);
#2802=EDGE_CURVE('',#2339,#2342,#1461,.T.);
#2803=EDGE_CURVE('',#2343,#2339,#1462,.T.);
#2804=EDGE_CURVE('',#2344,#2342,#1463,.T.);
#2805=EDGE_CURVE('',#2343,#2344,#1464,.T.);
#2806=EDGE_CURVE('',#2345,#2343,#1465,.T.);
#2807=EDGE_CURVE('',#2346,#2344,#1466,.T.);
#2808=EDGE_CURVE('',#2345,#2346,#1467,.T.);
#2809=EDGE_CURVE('',#2340,#2345,#1468,.T.);
#2810=EDGE_CURVE('',#2341,#2346,#1469,.T.);
#2811=EDGE_CURVE('',#2347,#2347,#2054,.T.);
#2812=EDGE_CURVE('',#2347,#2348,#1470,.T.);
#2813=EDGE_CURVE('',#2348,#2348,#2055,.T.);
#2814=EDGE_CURVE('',#2349,#2349,#2056,.T.);
#2815=EDGE_CURVE('',#2349,#2350,#1471,.T.);
#2816=EDGE_CURVE('',#2350,#2350,#2057,.T.);
#2817=EDGE_CURVE('',#2351,#2351,#2058,.T.);
#2818=EDGE_CURVE('',#2351,#2352,#1472,.T.);
#2819=EDGE_CURVE('',#2352,#2352,#2059,.T.);
#2820=EDGE_CURVE('',#2353,#2353,#2060,.T.);
#2821=EDGE_CURVE('',#2353,#2354,#1473,.T.);
#2822=EDGE_CURVE('',#2354,#2354,#2061,.T.);
#2823=EDGE_CURVE('',#2355,#2355,#2062,.T.);
#2824=EDGE_CURVE('',#2355,#2356,#1474,.T.);
#2825=EDGE_CURVE('',#2356,#2356,#2063,.T.);
#2826=EDGE_CURVE('',#2357,#2358,#1475,.T.);
#2827=EDGE_CURVE('',#2358,#2359,#1476,.T.);
#2828=EDGE_CURVE('',#2360,#2359,#1477,.T.);
#2829=EDGE_CURVE('',#2357,#2360,#1478,.T.);
#2830=EDGE_CURVE('',#2361,#2357,#1479,.T.);
#2831=EDGE_CURVE('',#2362,#2360,#1480,.T.);
#2832=EDGE_CURVE('',#2361,#2362,#1481,.T.);
#2833=EDGE_CURVE('',#2363,#2361,#1482,.T.);
#2834=EDGE_CURVE('',#2364,#2362,#1483,.T.);
#2835=EDGE_CURVE('',#2363,#2364,#1484,.T.);
#2836=EDGE_CURVE('',#2358,#2363,#1485,.T.);
#2837=EDGE_CURVE('',#2359,#2364,#1486,.T.);
#2838=EDGE_CURVE('',#2365,#2365,#2064,.T.);
#2839=EDGE_CURVE('',#2365,#2366,#1487,.T.);
#2840=EDGE_CURVE('',#2366,#2366,#2065,.T.);
#2841=EDGE_CURVE('',#2367,#2367,#2066,.T.);
#2842=EDGE_CURVE('',#2367,#2368,#1488,.T.);
#2843=EDGE_CURVE('',#2368,#2368,#2067,.T.);
#2844=EDGE_CURVE('',#2369,#2370,#2068,.T.);
#2845=EDGE_CURVE('',#2371,#2369,#1489,.T.);
#2846=EDGE_CURVE('',#2372,#2371,#1490,.T.);
#2847=EDGE_CURVE('',#2370,#2372,#1491,.T.);
#2848=EDGE_CURVE('',#2370,#2373,#1492,.T.);
#2849=EDGE_CURVE('',#2374,#2372,#1493,.T.);
#2850=EDGE_CURVE('',#2374,#2373,#1494,.T.);
#2851=EDGE_CURVE('',#2373,#2375,#2069,.T.);
#2852=EDGE_CURVE('',#2376,#2374,#1495,.T.);
#2853=EDGE_CURVE('',#2375,#2376,#1496,.T.);
#2854=EDGE_CURVE('',#2375,#2369,#1497,.T.);
#2855=EDGE_CURVE('',#2376,#2371,#1498,.T.);
#2856=EDGE_CURVE('',#2377,#2377,#2070,.T.);
#2857=EDGE_CURVE('',#2378,#2378,#2071,.T.);
#2858=EDGE_CURVE('',#2379,#2379,#2072,.T.);
#2859=EDGE_CURVE('',#2379,#2377,#1499,.T.);
#2860=EDGE_CURVE('',#2380,#2380,#2073,.T.);
#2861=EDGE_CURVE('',#2381,#2381,#2074,.T.);
#2862=EDGE_CURVE('',#2381,#2380,#1500,.T.);
#2863=EDGE_CURVE('',#2382,#2382,#2075,.T.);
#2864=EDGE_CURVE('',#2383,#2383,#2076,.T.);
#2865=EDGE_CURVE('',#2383,#2382,#1501,.T.);
#2866=EDGE_CURVE('',#2384,#2384,#2077,.T.);
#2867=EDGE_CURVE('',#2385,#2385,#2078,.T.);
#2868=EDGE_CURVE('',#2385,#2384,#1502,.T.);
#2869=EDGE_CURVE('',#2386,#2386,#2079,.T.);
#2870=EDGE_CURVE('',#2387,#2387,#2080,.T.);
#2871=EDGE_CURVE('',#2387,#2386,#1503,.T.);
#2872=EDGE_CURVE('',#2388,#2388,#2081,.T.);
#2873=EDGE_CURVE('',#2388,#2378,#1504,.T.);
#2874=EDGE_CURVE('',#2389,#2390,#2082,.T.);
#2875=EDGE_CURVE('',#2391,#2389,#1505,.T.);
#2876=EDGE_CURVE('',#2392,#2391,#2083,.T.);
#2877=EDGE_CURVE('',#2390,#2392,#1506,.T.);
#2878=EDGE_CURVE('',#2390,#2393,#1507,.T.);
#2879=EDGE_CURVE('',#2394,#2392,#1508,.T.);
#2880=EDGE_CURVE('',#2394,#2393,#1509,.T.);
#2881=EDGE_CURVE('',#2393,#2395,#2084,.T.);
#2882=EDGE_CURVE('',#2396,#2394,#2085,.T.);
#2883=EDGE_CURVE('',#2395,#2396,#1510,.T.);
#2884=EDGE_CURVE('',#2395,#2389,#1511,.T.);
#2885=EDGE_CURVE('',#2391,#2396,#1512,.T.);
#2886=EDGE_CURVE('',#2397,#2397,#2086,.T.);
#2887=EDGE_CURVE('',#2398,#2398,#2087,.T.);
#2888=EDGE_CURVE('',#2399,#2399,#2088,.T.);
#2889=EDGE_CURVE('',#2399,#2397,#1513,.T.);
#2890=EDGE_CURVE('',#2400,#2400,#2089,.T.);
#2891=EDGE_CURVE('',#2400,#2398,#1514,.T.);
#2892=EDGE_CURVE('',#2401,#2401,#2090,.T.);
#2893=EDGE_CURVE('',#2402,#2402,#2091,.T.);
#2894=EDGE_CURVE('',#2402,#2401,#1515,.T.);
#2895=EDGE_CURVE('',#2403,#2403,#2092,.T.);
#2896=EDGE_CURVE('',#2403,#2402,#1516,.T.);
#2897=EDGE_CURVE('',#2404,#2404,#2093,.T.);
#2898=EDGE_CURVE('',#2404,#2403,#1517,.T.);
#2899=EDGE_CURVE('',#2405,#2405,#2094,.T.);
#2900=EDGE_CURVE('',#2406,#2406,#2095,.F.);
#2901=EDGE_CURVE('',#2406,#2405,#1518,.T.);
#2902=EDGE_CURVE('',#2407,#2407,#2096,.F.);
#2903=EDGE_CURVE('',#2407,#2406,#1519,.T.);
#2904=EDGE_CURVE('',#2408,#2408,#2097,.T.);
#2905=EDGE_CURVE('',#2408,#2407,#1520,.T.);
#2906=EDGE_CURVE('',#2409,#2410,#1521,.T.);
#2907=EDGE_CURVE('',#2410,#2411,#1522,.T.);
#2908=EDGE_CURVE('',#2411,#2412,#1523,.T.);
#2909=EDGE_CURVE('',#2409,#2412,#1524,.T.);
#2910=EDGE_CURVE('',#2410,#2413,#1525,.T.);
#2911=EDGE_CURVE('',#2413,#2414,#1526,.T.);
#2912=EDGE_CURVE('',#2414,#2411,#1527,.T.);
#2913=EDGE_CURVE('',#2413,#2415,#1528,.T.);
#2914=EDGE_CURVE('',#2415,#2416,#1529,.T.);
#2915=EDGE_CURVE('',#2416,#2414,#1530,.T.);
#2916=EDGE_CURVE('',#2415,#2417,#1531,.T.);
#2917=EDGE_CURVE('',#2417,#2418,#1532,.T.);
#2918=EDGE_CURVE('',#2418,#2416,#1533,.T.);
#2919=EDGE_CURVE('',#2417,#2419,#1534,.T.);
#2920=EDGE_CURVE('',#2419,#2420,#1535,.T.);
#2921=EDGE_CURVE('',#2420,#2418,#1536,.T.);
#2922=EDGE_CURVE('',#2419,#2409,#1537,.T.);
#2923=EDGE_CURVE('',#2412,#2420,#1538,.T.);
#2924=EDGE_CURVE('',#2421,#2421,#2098,.T.);
#2925=EDGE_CURVE('',#2422,#2422,#2099,.T.);
#2926=EDGE_CURVE('',#2422,#2421,#1539,.T.);
#2927=EDGE_CURVE('',#2423,#2423,#2100,.T.);
#2928=EDGE_CURVE('',#2423,#2422,#1540,.T.);
#2929=EDGE_CURVE('',#2424,#2424,#2101,.T.);
#2930=EDGE_CURVE('',#2424,#2423,#1541,.T.);
#2931=EDGE_CURVE('',#2425,#2425,#2102,.T.);
#2932=EDGE_CURVE('',#2426,#2426,#2103,.F.);
#2933=EDGE_CURVE('',#2426,#2425,#1542,.T.);
#2934=EDGE_CURVE('',#2427,#2427,#2104,.F.);
#2935=EDGE_CURVE('',#2427,#2426,#1543,.T.);
#2936=EDGE_CURVE('',#2428,#2428,#2105,.T.);
#2937=EDGE_CURVE('',#2428,#2427,#1544,.T.);
#2938=EDGE_CURVE('',#2429,#2430,#1545,.T.);
#2939=EDGE_CURVE('',#2430,#2431,#1546,.T.);
#2940=EDGE_CURVE('',#2431,#2432,#1547,.T.);
#2941=EDGE_CURVE('',#2429,#2432,#1548,.T.);
#2942=EDGE_CURVE('',#2430,#2433,#1549,.T.);
#2943=EDGE_CURVE('',#2433,#2434,#1550,.T.);
#2944=EDGE_CURVE('',#2434,#2431,#1551,.T.);
#2945=EDGE_CURVE('',#2433,#2435,#1552,.T.);
#2946=EDGE_CURVE('',#2435,#2436,#1553,.T.);
#2947=EDGE_CURVE('',#2436,#2434,#1554,.T.);
#2948=EDGE_CURVE('',#2435,#2437,#1555,.T.);
#2949=EDGE_CURVE('',#2437,#2438,#1556,.T.);
#2950=EDGE_CURVE('',#2438,#2436,#1557,.T.);
#2951=EDGE_CURVE('',#2437,#2439,#1558,.T.);
#2952=EDGE_CURVE('',#2439,#2440,#1559,.T.);
#2953=EDGE_CURVE('',#2440,#2438,#1560,.T.);
#2954=EDGE_CURVE('',#2439,#2429,#1561,.T.);
#2955=EDGE_CURVE('',#2432,#2440,#1562,.T.);
#2956=EDGE_CURVE('',#2441,#2441,#2106,.T.);
#2957=EDGE_CURVE('',#2441,#2442,#1563,.T.);
#2958=EDGE_CURVE('',#2442,#2442,#2107,.T.);
#2959=EDGE_CURVE('',#2443,#2443,#2108,.T.);
#2960=EDGE_CURVE('',#2443,#2444,#1564,.T.);
#2961=EDGE_CURVE('',#2444,#2444,#2109,.T.);
#2962=EDGE_CURVE('',#2445,#2445,#2110,.T.);
#2963=EDGE_CURVE('',#2446,#2446,#2111,.T.);
#2964=EDGE_CURVE('',#2446,#2445,#1565,.T.);
#2965=EDGE_CURVE('',#2447,#2447,#2112,.T.);
#2966=EDGE_CURVE('',#2447,#2446,#1566,.T.);
#2967=EDGE_CURVE('',#2448,#2448,#2113,.T.);
#2968=EDGE_CURVE('',#2448,#2447,#1567,.T.);
#2969=EDGE_CURVE('',#2449,#2449,#2114,.T.);
#2970=EDGE_CURVE('',#2450,#2450,#2115,.F.);
#2971=EDGE_CURVE('',#2450,#2449,#1568,.T.);
#2972=EDGE_CURVE('',#2451,#2451,#2116,.F.);
#2973=EDGE_CURVE('',#2451,#2450,#1569,.T.);
#2974=EDGE_CURVE('',#2452,#2452,#2117,.T.);
#2975=EDGE_CURVE('',#2452,#2451,#1570,.T.);
#2976=EDGE_CURVE('',#2453,#2454,#1571,.T.);
#2977=EDGE_CURVE('',#2454,#2455,#1572,.T.);
#2978=EDGE_CURVE('',#2455,#2456,#1573,.T.);
#2979=EDGE_CURVE('',#2453,#2456,#1574,.T.);
#2980=EDGE_CURVE('',#2454,#2457,#1575,.T.);
#2981=EDGE_CURVE('',#2457,#2458,#1576,.T.);
#2982=EDGE_CURVE('',#2458,#2455,#1577,.T.);
#2983=EDGE_CURVE('',#2457,#2459,#1578,.T.);
#2984=EDGE_CURVE('',#2459,#2460,#1579,.T.);
#2985=EDGE_CURVE('',#2460,#2458,#1580,.T.);
#2986=EDGE_CURVE('',#2459,#2461,#1581,.T.);
#2987=EDGE_CURVE('',#2461,#2462,#1582,.T.);
#2988=EDGE_CURVE('',#2462,#2460,#1583,.T.);
#2989=EDGE_CURVE('',#2461,#2463,#1584,.T.);
#2990=EDGE_CURVE('',#2463,#2464,#1585,.T.);
#2991=EDGE_CURVE('',#2464,#2462,#1586,.T.);
#2992=EDGE_CURVE('',#2463,#2453,#1587,.T.);
#2993=EDGE_CURVE('',#2456,#2464,#1588,.T.);
#2994=ORIENTED_EDGE('',*,*,#2465,.F.);
#2995=ORIENTED_EDGE('',*,*,#2466,.T.);
#2996=ORIENTED_EDGE('',*,*,#2467,.F.);
#2997=ORIENTED_EDGE('',*,*,#2466,.F.);
#2998=ORIENTED_EDGE('',*,*,#2468,.F.);
#2999=ORIENTED_EDGE('',*,*,#2469,.T.);
#3000=ORIENTED_EDGE('',*,*,#2470,.F.);
#3001=ORIENTED_EDGE('',*,*,#2469,.F.);
#3002=ORIENTED_EDGE('',*,*,#2471,.F.);
#3003=ORIENTED_EDGE('',*,*,#2472,.T.);
#3004=ORIENTED_EDGE('',*,*,#2473,.F.);
#3005=ORIENTED_EDGE('',*,*,#2472,.F.);
#3006=ORIENTED_EDGE('',*,*,#2474,.F.);
#3007=ORIENTED_EDGE('',*,*,#2475,.T.);
#3008=ORIENTED_EDGE('',*,*,#2476,.F.);
#3009=ORIENTED_EDGE('',*,*,#2475,.F.);
#3010=ORIENTED_EDGE('',*,*,#2477,.F.);
#3011=ORIENTED_EDGE('',*,*,#2478,.T.);
#3012=ORIENTED_EDGE('',*,*,#2479,.F.);
#3013=ORIENTED_EDGE('',*,*,#2478,.F.);
#3014=ORIENTED_EDGE('',*,*,#2480,.F.);
#3015=ORIENTED_EDGE('',*,*,#2481,.T.);
#3016=ORIENTED_EDGE('',*,*,#2482,.F.);
#3017=ORIENTED_EDGE('',*,*,#2481,.F.);
#3018=ORIENTED_EDGE('',*,*,#2483,.F.);
#3019=ORIENTED_EDGE('',*,*,#2484,.T.);
#3020=ORIENTED_EDGE('',*,*,#2485,.F.);
#3021=ORIENTED_EDGE('',*,*,#2484,.F.);
#3022=ORIENTED_EDGE('',*,*,#2486,.F.);
#3023=ORIENTED_EDGE('',*,*,#2487,.T.);
#3024=ORIENTED_EDGE('',*,*,#2488,.F.);
#3025=ORIENTED_EDGE('',*,*,#2487,.F.);
#3026=ORIENTED_EDGE('',*,*,#2489,.F.);
#3027=ORIENTED_EDGE('',*,*,#2490,.T.);
#3028=ORIENTED_EDGE('',*,*,#2491,.F.);
#3029=ORIENTED_EDGE('',*,*,#2490,.F.);
#3030=ORIENTED_EDGE('',*,*,#2492,.F.);
#3031=ORIENTED_EDGE('',*,*,#2493,.T.);
#3032=ORIENTED_EDGE('',*,*,#2494,.F.);
#3033=ORIENTED_EDGE('',*,*,#2493,.F.);
#3034=ORIENTED_EDGE('',*,*,#2495,.F.);
#3035=ORIENTED_EDGE('',*,*,#2496,.T.);
#3036=ORIENTED_EDGE('',*,*,#2497,.F.);
#3037=ORIENTED_EDGE('',*,*,#2496,.F.);
#3038=ORIENTED_EDGE('',*,*,#2498,.F.);
#3039=ORIENTED_EDGE('',*,*,#2499,.T.);
#3040=ORIENTED_EDGE('',*,*,#2500,.F.);
#3041=ORIENTED_EDGE('',*,*,#2499,.F.);
#3042=ORIENTED_EDGE('',*,*,#2501,.T.);
#3043=ORIENTED_EDGE('',*,*,#2502,.T.);
#3044=ORIENTED_EDGE('',*,*,#2503,.F.);
#3045=ORIENTED_EDGE('',*,*,#2504,.F.);
#3046=ORIENTED_EDGE('',*,*,#2505,.T.);
#3047=ORIENTED_EDGE('',*,*,#2504,.T.);
#3048=ORIENTED_EDGE('',*,*,#2506,.F.);
#3049=ORIENTED_EDGE('',*,*,#2507,.F.);
#3050=ORIENTED_EDGE('',*,*,#2508,.T.);
#3051=ORIENTED_EDGE('',*,*,#2507,.T.);
#3052=ORIENTED_EDGE('',*,*,#2509,.F.);
#3053=ORIENTED_EDGE('',*,*,#2510,.F.);
#3054=ORIENTED_EDGE('',*,*,#2511,.T.);
#3055=ORIENTED_EDGE('',*,*,#2510,.T.);
#3056=ORIENTED_EDGE('',*,*,#2512,.F.);
#3057=ORIENTED_EDGE('',*,*,#2502,.F.);
#3058=ORIENTED_EDGE('',*,*,#2512,.T.);
#3059=ORIENTED_EDGE('',*,*,#2509,.T.);
#3060=ORIENTED_EDGE('',*,*,#2506,.T.);
#3061=ORIENTED_EDGE('',*,*,#2503,.T.);
#3062=ORIENTED_EDGE('',*,*,#2479,.T.);
#3063=ORIENTED_EDGE('',*,*,#2482,.T.);
#3064=ORIENTED_EDGE('',*,*,#2485,.T.);
#3065=ORIENTED_EDGE('',*,*,#2488,.T.);
#3066=ORIENTED_EDGE('',*,*,#2491,.T.);
#3067=ORIENTED_EDGE('',*,*,#2494,.T.);
#3068=ORIENTED_EDGE('',*,*,#2497,.T.);
#3069=ORIENTED_EDGE('',*,*,#2500,.T.);
#3070=ORIENTED_EDGE('',*,*,#2476,.T.);
#3071=ORIENTED_EDGE('',*,*,#2473,.T.);
#3072=ORIENTED_EDGE('',*,*,#2470,.T.);
#3073=ORIENTED_EDGE('',*,*,#2467,.T.);
#3074=ORIENTED_EDGE('',*,*,#2511,.F.);
#3075=ORIENTED_EDGE('',*,*,#2501,.F.);
#3076=ORIENTED_EDGE('',*,*,#2505,.F.);
#3077=ORIENTED_EDGE('',*,*,#2508,.F.);
#3078=ORIENTED_EDGE('',*,*,#2477,.T.);
#3079=ORIENTED_EDGE('',*,*,#2480,.T.);
#3080=ORIENTED_EDGE('',*,*,#2483,.T.);
#3081=ORIENTED_EDGE('',*,*,#2486,.T.);
#3082=ORIENTED_EDGE('',*,*,#2489,.T.);
#3083=ORIENTED_EDGE('',*,*,#2492,.T.);
#3084=ORIENTED_EDGE('',*,*,#2495,.T.);
#3085=ORIENTED_EDGE('',*,*,#2498,.T.);
#3086=ORIENTED_EDGE('',*,*,#2474,.T.);
#3087=ORIENTED_EDGE('',*,*,#2471,.T.);
#3088=ORIENTED_EDGE('',*,*,#2468,.T.);
#3089=ORIENTED_EDGE('',*,*,#2465,.T.);
#3090=ORIENTED_EDGE('',*,*,#2513,.F.);
#3091=ORIENTED_EDGE('',*,*,#2514,.T.);
#3092=ORIENTED_EDGE('',*,*,#2515,.F.);
#3093=ORIENTED_EDGE('',*,*,#2514,.F.);
#3094=ORIENTED_EDGE('',*,*,#2513,.T.);
#3095=ORIENTED_EDGE('',*,*,#2516,.F.);
#3096=ORIENTED_EDGE('',*,*,#2517,.F.);
#3097=ORIENTED_EDGE('',*,*,#2518,.T.);
#3098=ORIENTED_EDGE('',*,*,#2519,.F.);
#3099=ORIENTED_EDGE('',*,*,#2518,.F.);
#3100=ORIENTED_EDGE('',*,*,#2517,.T.);
#3101=ORIENTED_EDGE('',*,*,#2520,.F.);
#3102=ORIENTED_EDGE('',*,*,#2521,.F.);
#3103=ORIENTED_EDGE('',*,*,#2522,.T.);
#3104=ORIENTED_EDGE('',*,*,#2516,.T.);
#3105=ORIENTED_EDGE('',*,*,#2522,.F.);
#3106=ORIENTED_EDGE('',*,*,#2523,.F.);
#3107=ORIENTED_EDGE('',*,*,#2524,.T.);
#3108=ORIENTED_EDGE('',*,*,#2520,.T.);
#3109=ORIENTED_EDGE('',*,*,#2524,.F.);
#3110=ORIENTED_EDGE('',*,*,#2525,.T.);
#3111=ORIENTED_EDGE('',*,*,#2526,.T.);
#3112=ORIENTED_EDGE('',*,*,#2527,.F.);
#3113=ORIENTED_EDGE('',*,*,#2528,.F.);
#3114=ORIENTED_EDGE('',*,*,#2529,.T.);
#3115=ORIENTED_EDGE('',*,*,#2528,.T.);
#3116=ORIENTED_EDGE('',*,*,#2530,.F.);
#3117=ORIENTED_EDGE('',*,*,#2531,.F.);
#3118=ORIENTED_EDGE('',*,*,#2532,.T.);
#3119=ORIENTED_EDGE('',*,*,#2531,.T.);
#3120=ORIENTED_EDGE('',*,*,#2533,.F.);
#3121=ORIENTED_EDGE('',*,*,#2534,.F.);
#3122=ORIENTED_EDGE('',*,*,#2535,.T.);
#3123=ORIENTED_EDGE('',*,*,#2534,.T.);
#3124=ORIENTED_EDGE('',*,*,#2536,.F.);
#3125=ORIENTED_EDGE('',*,*,#2526,.F.);
#3126=ORIENTED_EDGE('',*,*,#2536,.T.);
#3127=ORIENTED_EDGE('',*,*,#2533,.T.);
#3128=ORIENTED_EDGE('',*,*,#2530,.T.);
#3129=ORIENTED_EDGE('',*,*,#2527,.T.);
#3130=ORIENTED_EDGE('',*,*,#2515,.T.);
#3131=ORIENTED_EDGE('',*,*,#2519,.T.);
#3132=ORIENTED_EDGE('',*,*,#2535,.F.);
#3133=ORIENTED_EDGE('',*,*,#2525,.F.);
#3134=ORIENTED_EDGE('',*,*,#2529,.F.);
#3135=ORIENTED_EDGE('',*,*,#2532,.F.);
#3136=ORIENTED_EDGE('',*,*,#2521,.T.);
#3137=ORIENTED_EDGE('',*,*,#2523,.T.);
#3138=ORIENTED_EDGE('',*,*,#2537,.T.);
#3139=ORIENTED_EDGE('',*,*,#2538,.T.);
#3140=ORIENTED_EDGE('',*,*,#2539,.F.);
#3141=ORIENTED_EDGE('',*,*,#2540,.F.);
#3142=ORIENTED_EDGE('',*,*,#2541,.T.);
#3143=ORIENTED_EDGE('',*,*,#2540,.T.);
#3144=ORIENTED_EDGE('',*,*,#2542,.F.);
#3145=ORIENTED_EDGE('',*,*,#2543,.F.);
#3146=ORIENTED_EDGE('',*,*,#2544,.T.);
#3147=ORIENTED_EDGE('',*,*,#2543,.T.);
#3148=ORIENTED_EDGE('',*,*,#2545,.F.);
#3149=ORIENTED_EDGE('',*,*,#2546,.F.);
#3150=ORIENTED_EDGE('',*,*,#2547,.T.);
#3151=ORIENTED_EDGE('',*,*,#2546,.T.);
#3152=ORIENTED_EDGE('',*,*,#2548,.F.);
#3153=ORIENTED_EDGE('',*,*,#2538,.F.);
#3154=ORIENTED_EDGE('',*,*,#2548,.T.);
#3155=ORIENTED_EDGE('',*,*,#2545,.T.);
#3156=ORIENTED_EDGE('',*,*,#2542,.T.);
#3157=ORIENTED_EDGE('',*,*,#2539,.T.);
#3158=ORIENTED_EDGE('',*,*,#2547,.F.);
#3159=ORIENTED_EDGE('',*,*,#2537,.F.);
#3160=ORIENTED_EDGE('',*,*,#2541,.F.);
#3161=ORIENTED_EDGE('',*,*,#2544,.F.);
#3162=ORIENTED_EDGE('',*,*,#2549,.F.);
#3163=ORIENTED_EDGE('',*,*,#2550,.T.);
#3164=ORIENTED_EDGE('',*,*,#2551,.F.);
#3165=ORIENTED_EDGE('',*,*,#2550,.F.);
#3166=ORIENTED_EDGE('',*,*,#2549,.T.);
#3167=ORIENTED_EDGE('',*,*,#2552,.F.);
#3168=ORIENTED_EDGE('',*,*,#2553,.F.);
#3169=ORIENTED_EDGE('',*,*,#2554,.T.);
#3170=ORIENTED_EDGE('',*,*,#2555,.F.);
#3171=ORIENTED_EDGE('',*,*,#2554,.F.);
#3172=ORIENTED_EDGE('',*,*,#2553,.T.);
#3173=ORIENTED_EDGE('',*,*,#2556,.F.);
#3174=ORIENTED_EDGE('',*,*,#2557,.F.);
#3175=ORIENTED_EDGE('',*,*,#2558,.T.);
#3176=ORIENTED_EDGE('',*,*,#2552,.T.);
#3177=ORIENTED_EDGE('',*,*,#2558,.F.);
#3178=ORIENTED_EDGE('',*,*,#2559,.F.);
#3179=ORIENTED_EDGE('',*,*,#2560,.T.);
#3180=ORIENTED_EDGE('',*,*,#2556,.T.);
#3181=ORIENTED_EDGE('',*,*,#2560,.F.);
#3182=ORIENTED_EDGE('',*,*,#2561,.T.);
#3183=ORIENTED_EDGE('',*,*,#2562,.T.);
#3184=ORIENTED_EDGE('',*,*,#2563,.F.);
#3185=ORIENTED_EDGE('',*,*,#2564,.F.);
#3186=ORIENTED_EDGE('',*,*,#2565,.T.);
#3187=ORIENTED_EDGE('',*,*,#2564,.T.);
#3188=ORIENTED_EDGE('',*,*,#2566,.F.);
#3189=ORIENTED_EDGE('',*,*,#2567,.F.);
#3190=ORIENTED_EDGE('',*,*,#2568,.T.);
#3191=ORIENTED_EDGE('',*,*,#2567,.T.);
#3192=ORIENTED_EDGE('',*,*,#2569,.F.);
#3193=ORIENTED_EDGE('',*,*,#2570,.F.);
#3194=ORIENTED_EDGE('',*,*,#2571,.T.);
#3195=ORIENTED_EDGE('',*,*,#2570,.T.);
#3196=ORIENTED_EDGE('',*,*,#2572,.F.);
#3197=ORIENTED_EDGE('',*,*,#2562,.F.);
#3198=ORIENTED_EDGE('',*,*,#2572,.T.);
#3199=ORIENTED_EDGE('',*,*,#2569,.T.);
#3200=ORIENTED_EDGE('',*,*,#2566,.T.);
#3201=ORIENTED_EDGE('',*,*,#2563,.T.);
#3202=ORIENTED_EDGE('',*,*,#2551,.T.);
#3203=ORIENTED_EDGE('',*,*,#2555,.T.);
#3204=ORIENTED_EDGE('',*,*,#2571,.F.);
#3205=ORIENTED_EDGE('',*,*,#2561,.F.);
#3206=ORIENTED_EDGE('',*,*,#2565,.F.);
#3207=ORIENTED_EDGE('',*,*,#2568,.F.);
#3208=ORIENTED_EDGE('',*,*,#2557,.T.);
#3209=ORIENTED_EDGE('',*,*,#2559,.T.);
#3210=ORIENTED_EDGE('',*,*,#2573,.T.);
#3211=ORIENTED_EDGE('',*,*,#2574,.T.);
#3212=ORIENTED_EDGE('',*,*,#2575,.F.);
#3213=ORIENTED_EDGE('',*,*,#2576,.F.);
#3214=ORIENTED_EDGE('',*,*,#2577,.T.);
#3215=ORIENTED_EDGE('',*,*,#2576,.T.);
#3216=ORIENTED_EDGE('',*,*,#2578,.F.);
#3217=ORIENTED_EDGE('',*,*,#2579,.F.);
#3218=ORIENTED_EDGE('',*,*,#2580,.T.);
#3219=ORIENTED_EDGE('',*,*,#2579,.T.);
#3220=ORIENTED_EDGE('',*,*,#2581,.F.);
#3221=ORIENTED_EDGE('',*,*,#2582,.F.);
#3222=ORIENTED_EDGE('',*,*,#2583,.T.);
#3223=ORIENTED_EDGE('',*,*,#2582,.T.);
#3224=ORIENTED_EDGE('',*,*,#2584,.F.);
#3225=ORIENTED_EDGE('',*,*,#2574,.F.);
#3226=ORIENTED_EDGE('',*,*,#2584,.T.);
#3227=ORIENTED_EDGE('',*,*,#2581,.T.);
#3228=ORIENTED_EDGE('',*,*,#2578,.T.);
#3229=ORIENTED_EDGE('',*,*,#2575,.T.);
#3230=ORIENTED_EDGE('',*,*,#2583,.F.);
#3231=ORIENTED_EDGE('',*,*,#2573,.F.);
#3232=ORIENTED_EDGE('',*,*,#2577,.F.);
#3233=ORIENTED_EDGE('',*,*,#2580,.F.);
#3234=ORIENTED_EDGE('',*,*,#2585,.T.);
#3235=ORIENTED_EDGE('',*,*,#2586,.T.);
#3236=ORIENTED_EDGE('',*,*,#2587,.T.);
#3237=ORIENTED_EDGE('',*,*,#2586,.F.);
#3238=ORIENTED_EDGE('',*,*,#2588,.F.);
#3239=ORIENTED_EDGE('',*,*,#2589,.T.);
#3240=ORIENTED_EDGE('',*,*,#2585,.F.);
#3241=ORIENTED_EDGE('',*,*,#2589,.F.);
#3242=ORIENTED_EDGE('',*,*,#2587,.F.);
#3243=ORIENTED_EDGE('',*,*,#2590,.T.);
#3244=ORIENTED_EDGE('',*,*,#2591,.T.);
#3245=ORIENTED_EDGE('',*,*,#2588,.T.);
#3246=ORIENTED_EDGE('',*,*,#2591,.F.);
#3247=ORIENTED_EDGE('',*,*,#2590,.F.);
#3248=ORIENTED_EDGE('',*,*,#2592,.F.);
#3249=ORIENTED_EDGE('',*,*,#2593,.F.);
#3250=ORIENTED_EDGE('',*,*,#2594,.F.);
#3251=ORIENTED_EDGE('',*,*,#2595,.F.);
#3252=ORIENTED_EDGE('',*,*,#2596,.F.);
#3253=ORIENTED_EDGE('',*,*,#2593,.T.);
#3254=ORIENTED_EDGE('',*,*,#2597,.F.);
#3255=ORIENTED_EDGE('',*,*,#2598,.T.);
#3256=ORIENTED_EDGE('',*,*,#2599,.F.);
#3257=ORIENTED_EDGE('',*,*,#2600,.F.);
#3258=ORIENTED_EDGE('',*,*,#2601,.F.);
#3259=ORIENTED_EDGE('',*,*,#2598,.F.);
#3260=ORIENTED_EDGE('',*,*,#2602,.T.);
#3261=ORIENTED_EDGE('',*,*,#2603,.F.);
#3262=ORIENTED_EDGE('',*,*,#2604,.T.);
#3263=ORIENTED_EDGE('',*,*,#2605,.F.);
#3264=ORIENTED_EDGE('',*,*,#2606,.T.);
#3265=ORIENTED_EDGE('',*,*,#2595,.T.);
#3266=ORIENTED_EDGE('',*,*,#2607,.T.);
#3267=ORIENTED_EDGE('',*,*,#2594,.T.);
#3268=ORIENTED_EDGE('',*,*,#2592,.T.);
#3269=ORIENTED_EDGE('',*,*,#2596,.T.);
#3270=ORIENTED_EDGE('',*,*,#2606,.F.);
#3271=ORIENTED_EDGE('',*,*,#2608,.F.);
#3272=ORIENTED_EDGE('',*,*,#2609,.T.);
#3273=ORIENTED_EDGE('',*,*,#2610,.F.);
#3274=ORIENTED_EDGE('',*,*,#2602,.F.);
#3275=ORIENTED_EDGE('',*,*,#2611,.T.);
#3276=ORIENTED_EDGE('',*,*,#2612,.T.);
#3277=ORIENTED_EDGE('',*,*,#2613,.F.);
#3278=ORIENTED_EDGE('',*,*,#2614,.F.);
#3279=ORIENTED_EDGE('',*,*,#2600,.T.);
#3280=ORIENTED_EDGE('',*,*,#2615,.F.);
#3281=ORIENTED_EDGE('',*,*,#2616,.F.);
#3282=ORIENTED_EDGE('',*,*,#2617,.T.);
#3283=ORIENTED_EDGE('',*,*,#2618,.F.);
#3284=ORIENTED_EDGE('',*,*,#2619,.T.);
#3285=ORIENTED_EDGE('',*,*,#2620,.F.);
#3286=ORIENTED_EDGE('',*,*,#2619,.F.);
#3287=ORIENTED_EDGE('',*,*,#2611,.F.);
#3288=ORIENTED_EDGE('',*,*,#2621,.T.);
#3289=ORIENTED_EDGE('',*,*,#2622,.F.);
#3290=ORIENTED_EDGE('',*,*,#2621,.F.);
#3291=ORIENTED_EDGE('',*,*,#2623,.F.);
#3292=ORIENTED_EDGE('',*,*,#2624,.T.);
#3293=ORIENTED_EDGE('',*,*,#2607,.F.);
#3294=ORIENTED_EDGE('',*,*,#2624,.F.);
#3295=ORIENTED_EDGE('',*,*,#2625,.F.);
#3296=ORIENTED_EDGE('',*,*,#2626,.T.);
#3297=ORIENTED_EDGE('',*,*,#2617,.F.);
#3298=ORIENTED_EDGE('',*,*,#2626,.F.);
#3299=ORIENTED_EDGE('',*,*,#2627,.F.);
#3300=ORIENTED_EDGE('',*,*,#2628,.T.);
#3301=ORIENTED_EDGE('',*,*,#2629,.F.);
#3302=ORIENTED_EDGE('',*,*,#2628,.F.);
#3303=ORIENTED_EDGE('',*,*,#2605,.T.);
#3304=ORIENTED_EDGE('',*,*,#2630,.T.);
#3305=ORIENTED_EDGE('',*,*,#2631,.T.);
#3306=ORIENTED_EDGE('',*,*,#2632,.T.);
#3307=ORIENTED_EDGE('',*,*,#2616,.T.);
#3308=ORIENTED_EDGE('',*,*,#2633,.T.);
#3309=ORIENTED_EDGE('',*,*,#2634,.T.);
#3310=ORIENTED_EDGE('',*,*,#2635,.T.);
#3311=ORIENTED_EDGE('',*,*,#2636,.T.);
#3312=ORIENTED_EDGE('',*,*,#2637,.T.);
#3313=ORIENTED_EDGE('',*,*,#2638,.T.);
#3314=ORIENTED_EDGE('',*,*,#2608,.T.);
#3315=ORIENTED_EDGE('',*,*,#2627,.T.);
#3316=ORIENTED_EDGE('',*,*,#2604,.F.);
#3317=ORIENTED_EDGE('',*,*,#2639,.F.);
#3318=ORIENTED_EDGE('',*,*,#2640,.F.);
#3319=ORIENTED_EDGE('',*,*,#2630,.F.);
#3320=ORIENTED_EDGE('',*,*,#2640,.T.);
#3321=ORIENTED_EDGE('',*,*,#2641,.F.);
#3322=ORIENTED_EDGE('',*,*,#2642,.F.);
#3323=ORIENTED_EDGE('',*,*,#2631,.F.);
#3324=ORIENTED_EDGE('',*,*,#2623,.T.);
#3325=ORIENTED_EDGE('',*,*,#2625,.T.);
#3326=ORIENTED_EDGE('',*,*,#2642,.T.);
#3327=ORIENTED_EDGE('',*,*,#2643,.F.);
#3328=ORIENTED_EDGE('',*,*,#2612,.F.);
#3329=ORIENTED_EDGE('',*,*,#2632,.F.);
#3330=ORIENTED_EDGE('',*,*,#2597,.T.);
#3331=ORIENTED_EDGE('',*,*,#2614,.T.);
#3332=ORIENTED_EDGE('',*,*,#2644,.F.);
#3333=ORIENTED_EDGE('',*,*,#2645,.F.);
#3334=ORIENTED_EDGE('',*,*,#2633,.F.);
#3335=ORIENTED_EDGE('',*,*,#2615,.T.);
#3336=ORIENTED_EDGE('',*,*,#2599,.T.);
#3337=ORIENTED_EDGE('',*,*,#2601,.T.);
#3338=ORIENTED_EDGE('',*,*,#2620,.T.);
#3339=ORIENTED_EDGE('',*,*,#2645,.T.);
#3340=ORIENTED_EDGE('',*,*,#2646,.F.);
#3341=ORIENTED_EDGE('',*,*,#2647,.F.);
#3342=ORIENTED_EDGE('',*,*,#2634,.F.);
#3343=ORIENTED_EDGE('',*,*,#2647,.T.);
#3344=ORIENTED_EDGE('',*,*,#2648,.F.);
#3345=ORIENTED_EDGE('',*,*,#2649,.F.);
#3346=ORIENTED_EDGE('',*,*,#2635,.F.);
#3347=ORIENTED_EDGE('',*,*,#2618,.T.);
#3348=ORIENTED_EDGE('',*,*,#2649,.T.);
#3349=ORIENTED_EDGE('',*,*,#2650,.F.);
#3350=ORIENTED_EDGE('',*,*,#2651,.F.);
#3351=ORIENTED_EDGE('',*,*,#2636,.F.);
#3352=ORIENTED_EDGE('',*,*,#2651,.T.);
#3353=ORIENTED_EDGE('',*,*,#2652,.F.);
#3354=ORIENTED_EDGE('',*,*,#2653,.F.);
#3355=ORIENTED_EDGE('',*,*,#2637,.F.);
#3356=ORIENTED_EDGE('',*,*,#2622,.T.);
#3357=ORIENTED_EDGE('',*,*,#2653,.T.);
#3358=ORIENTED_EDGE('',*,*,#2654,.F.);
#3359=ORIENTED_EDGE('',*,*,#2609,.F.);
#3360=ORIENTED_EDGE('',*,*,#2638,.F.);
#3361=ORIENTED_EDGE('',*,*,#2603,.T.);
#3362=ORIENTED_EDGE('',*,*,#2610,.T.);
#3363=ORIENTED_EDGE('',*,*,#2654,.T.);
#3364=ORIENTED_EDGE('',*,*,#2652,.T.);
#3365=ORIENTED_EDGE('',*,*,#2650,.T.);
#3366=ORIENTED_EDGE('',*,*,#2648,.T.);
#3367=ORIENTED_EDGE('',*,*,#2646,.T.);
#3368=ORIENTED_EDGE('',*,*,#2644,.T.);
#3369=ORIENTED_EDGE('',*,*,#2613,.T.);
#3370=ORIENTED_EDGE('',*,*,#2643,.T.);
#3371=ORIENTED_EDGE('',*,*,#2641,.T.);
#3372=ORIENTED_EDGE('',*,*,#2639,.T.);
#3373=ORIENTED_EDGE('',*,*,#2629,.T.);
#3374=ORIENTED_EDGE('',*,*,#2655,.T.);
#3375=ORIENTED_EDGE('',*,*,#2656,.T.);
#3376=ORIENTED_EDGE('',*,*,#2657,.T.);
#3377=ORIENTED_EDGE('',*,*,#2658,.F.);
#3378=ORIENTED_EDGE('',*,*,#2659,.T.);
#3379=ORIENTED_EDGE('',*,*,#2660,.T.);
#3380=ORIENTED_EDGE('',*,*,#2661,.T.);
#3381=ORIENTED_EDGE('',*,*,#2656,.F.);
#3382=ORIENTED_EDGE('',*,*,#2662,.T.);
#3383=ORIENTED_EDGE('',*,*,#2663,.T.);
#3384=ORIENTED_EDGE('',*,*,#2664,.T.);
#3385=ORIENTED_EDGE('',*,*,#2660,.F.);
#3386=ORIENTED_EDGE('',*,*,#2665,.T.);
#3387=ORIENTED_EDGE('',*,*,#2666,.T.);
#3388=ORIENTED_EDGE('',*,*,#2667,.T.);
#3389=ORIENTED_EDGE('',*,*,#2663,.F.);
#3390=ORIENTED_EDGE('',*,*,#2668,.T.);
#3391=ORIENTED_EDGE('',*,*,#2669,.T.);
#3392=ORIENTED_EDGE('',*,*,#2670,.T.);
#3393=ORIENTED_EDGE('',*,*,#2666,.F.);
#3394=ORIENTED_EDGE('',*,*,#2671,.T.);
#3395=ORIENTED_EDGE('',*,*,#2658,.T.);
#3396=ORIENTED_EDGE('',*,*,#2672,.T.);
#3397=ORIENTED_EDGE('',*,*,#2669,.F.);
#3398=ORIENTED_EDGE('',*,*,#2671,.F.);
#3399=ORIENTED_EDGE('',*,*,#2668,.F.);
#3400=ORIENTED_EDGE('',*,*,#2665,.F.);
#3401=ORIENTED_EDGE('',*,*,#2662,.F.);
#3402=ORIENTED_EDGE('',*,*,#2659,.F.);
#3403=ORIENTED_EDGE('',*,*,#2655,.F.);
#3404=ORIENTED_EDGE('',*,*,#2672,.F.);
#3405=ORIENTED_EDGE('',*,*,#2657,.F.);
#3406=ORIENTED_EDGE('',*,*,#2661,.F.);
#3407=ORIENTED_EDGE('',*,*,#2664,.F.);
#3408=ORIENTED_EDGE('',*,*,#2667,.F.);
#3409=ORIENTED_EDGE('',*,*,#2670,.F.);
#3410=ORIENTED_EDGE('',*,*,#2673,.F.);
#3411=ORIENTED_EDGE('',*,*,#2674,.F.);
#3412=ORIENTED_EDGE('',*,*,#2675,.F.);
#3413=ORIENTED_EDGE('',*,*,#2676,.T.);
#3414=ORIENTED_EDGE('',*,*,#2674,.T.);
#3415=ORIENTED_EDGE('',*,*,#2676,.F.);
#3416=ORIENTED_EDGE('',*,*,#2677,.F.);
#3417=ORIENTED_EDGE('',*,*,#2678,.T.);
#3418=ORIENTED_EDGE('',*,*,#2675,.T.);
#3419=ORIENTED_EDGE('',*,*,#2678,.F.);
#3420=ORIENTED_EDGE('',*,*,#2679,.F.);
#3421=ORIENTED_EDGE('',*,*,#2680,.T.);
#3422=ORIENTED_EDGE('',*,*,#2677,.T.);
#3423=ORIENTED_EDGE('',*,*,#2680,.F.);
#3424=ORIENTED_EDGE('',*,*,#2679,.T.);
#3425=ORIENTED_EDGE('',*,*,#2681,.F.);
#3426=ORIENTED_EDGE('',*,*,#2682,.F.);
#3427=ORIENTED_EDGE('',*,*,#2683,.T.);
#3428=ORIENTED_EDGE('',*,*,#2681,.T.);
#3429=ORIENTED_EDGE('',*,*,#2683,.F.);
#3430=ORIENTED_EDGE('',*,*,#2673,.T.);
#3431=ORIENTED_EDGE('',*,*,#2684,.T.);
#3432=ORIENTED_EDGE('',*,*,#2682,.T.);
#3433=ORIENTED_EDGE('',*,*,#2684,.F.);
#3434=ORIENTED_EDGE('',*,*,#2685,.F.);
#3435=ORIENTED_EDGE('',*,*,#2686,.T.);
#3436=ORIENTED_EDGE('',*,*,#2687,.F.);
#3437=ORIENTED_EDGE('',*,*,#2686,.F.);
#3438=ORIENTED_EDGE('',*,*,#2685,.T.);
#3439=ORIENTED_EDGE('',*,*,#2688,.F.);
#3440=ORIENTED_EDGE('',*,*,#2689,.T.);
#3441=ORIENTED_EDGE('',*,*,#2690,.F.);
#3442=ORIENTED_EDGE('',*,*,#2689,.F.);
#3443=ORIENTED_EDGE('',*,*,#2688,.T.);
#3444=ORIENTED_EDGE('',*,*,#2691,.F.);
#3445=ORIENTED_EDGE('',*,*,#2692,.T.);
#3446=ORIENTED_EDGE('',*,*,#2693,.F.);
#3447=ORIENTED_EDGE('',*,*,#2692,.F.);
#3448=ORIENTED_EDGE('',*,*,#2691,.T.);
#3449=ORIENTED_EDGE('',*,*,#2694,.F.);
#3450=ORIENTED_EDGE('',*,*,#2695,.T.);
#3451=ORIENTED_EDGE('',*,*,#2696,.F.);
#3452=ORIENTED_EDGE('',*,*,#2695,.F.);
#3453=ORIENTED_EDGE('',*,*,#2694,.T.);
#3454=ORIENTED_EDGE('',*,*,#2697,.F.);
#3455=ORIENTED_EDGE('',*,*,#2698,.T.);
#3456=ORIENTED_EDGE('',*,*,#2699,.T.);
#3457=ORIENTED_EDGE('',*,*,#2698,.F.);
#3458=ORIENTED_EDGE('',*,*,#2699,.F.);
#3459=ORIENTED_EDGE('',*,*,#2700,.F.);
#3460=ORIENTED_EDGE('',*,*,#2701,.T.);
#3461=ORIENTED_EDGE('',*,*,#2702,.T.);
#3462=ORIENTED_EDGE('',*,*,#2701,.F.);
#3463=ORIENTED_EDGE('',*,*,#2702,.F.);
#3464=ORIENTED_EDGE('',*,*,#2703,.F.);
#3465=ORIENTED_EDGE('',*,*,#2704,.T.);
#3466=ORIENTED_EDGE('',*,*,#2705,.T.);
#3467=ORIENTED_EDGE('',*,*,#2704,.F.);
#3468=ORIENTED_EDGE('',*,*,#2705,.F.);
#3469=ORIENTED_EDGE('',*,*,#2706,.F.);
#3470=ORIENTED_EDGE('',*,*,#2707,.T.);
#3471=ORIENTED_EDGE('',*,*,#2708,.T.);
#3472=ORIENTED_EDGE('',*,*,#2707,.F.);
#3473=ORIENTED_EDGE('',*,*,#2708,.F.);
#3474=ORIENTED_EDGE('',*,*,#2709,.F.);
#3475=ORIENTED_EDGE('',*,*,#2710,.T.);
#3476=ORIENTED_EDGE('',*,*,#2711,.F.);
#3477=ORIENTED_EDGE('',*,*,#2710,.F.);
#3478=ORIENTED_EDGE('',*,*,#2709,.T.);
#3479=ORIENTED_EDGE('',*,*,#2712,.F.);
#3480=ORIENTED_EDGE('',*,*,#2713,.T.);
#3481=ORIENTED_EDGE('',*,*,#2714,.F.);
#3482=ORIENTED_EDGE('',*,*,#2713,.F.);
#3483=ORIENTED_EDGE('',*,*,#2712,.T.);
#3484=ORIENTED_EDGE('',*,*,#2715,.F.);
#3485=ORIENTED_EDGE('',*,*,#2716,.T.);
#3486=ORIENTED_EDGE('',*,*,#2717,.F.);
#3487=ORIENTED_EDGE('',*,*,#2716,.F.);
#3488=ORIENTED_EDGE('',*,*,#2715,.T.);
#3489=ORIENTED_EDGE('',*,*,#2718,.F.);
#3490=ORIENTED_EDGE('',*,*,#2719,.T.);
#3491=ORIENTED_EDGE('',*,*,#2720,.F.);
#3492=ORIENTED_EDGE('',*,*,#2719,.F.);
#3493=ORIENTED_EDGE('',*,*,#2718,.T.);
#3494=ORIENTED_EDGE('',*,*,#2721,.F.);
#3495=ORIENTED_EDGE('',*,*,#2722,.T.);
#3496=ORIENTED_EDGE('',*,*,#2723,.F.);
#3497=ORIENTED_EDGE('',*,*,#2722,.F.);
#3498=ORIENTED_EDGE('',*,*,#2724,.F.);
#3499=ORIENTED_EDGE('',*,*,#2725,.T.);
#3500=ORIENTED_EDGE('',*,*,#2726,.F.);
#3501=ORIENTED_EDGE('',*,*,#2725,.F.);
#3502=ORIENTED_EDGE('',*,*,#2727,.T.);
#3503=ORIENTED_EDGE('',*,*,#2728,.T.);
#3504=ORIENTED_EDGE('',*,*,#2729,.F.);
#3505=ORIENTED_EDGE('',*,*,#2730,.F.);
#3506=ORIENTED_EDGE('',*,*,#2731,.T.);
#3507=ORIENTED_EDGE('',*,*,#2730,.T.);
#3508=ORIENTED_EDGE('',*,*,#2732,.F.);
#3509=ORIENTED_EDGE('',*,*,#2733,.F.);
#3510=ORIENTED_EDGE('',*,*,#2726,.T.);
#3511=ORIENTED_EDGE('',*,*,#2723,.T.);
#3512=ORIENTED_EDGE('',*,*,#2696,.T.);
#3513=ORIENTED_EDGE('',*,*,#2693,.T.);
#3514=ORIENTED_EDGE('',*,*,#2690,.T.);
#3515=ORIENTED_EDGE('',*,*,#2687,.T.);
#3516=ORIENTED_EDGE('',*,*,#2734,.T.);
#3517=ORIENTED_EDGE('',*,*,#2733,.T.);
#3518=ORIENTED_EDGE('',*,*,#2735,.F.);
#3519=ORIENTED_EDGE('',*,*,#2736,.F.);
#3520=ORIENTED_EDGE('',*,*,#2737,.T.);
#3521=ORIENTED_EDGE('',*,*,#2736,.T.);
#3522=ORIENTED_EDGE('',*,*,#2738,.F.);
#3523=ORIENTED_EDGE('',*,*,#2728,.F.);
#3524=ORIENTED_EDGE('',*,*,#2724,.T.);
#3525=ORIENTED_EDGE('',*,*,#2721,.T.);
#3526=ORIENTED_EDGE('',*,*,#2706,.T.);
#3527=ORIENTED_EDGE('',*,*,#2703,.T.);
#3528=ORIENTED_EDGE('',*,*,#2700,.T.);
#3529=ORIENTED_EDGE('',*,*,#2697,.T.);
#3530=ORIENTED_EDGE('',*,*,#2738,.T.);
#3531=ORIENTED_EDGE('',*,*,#2735,.T.);
#3532=ORIENTED_EDGE('',*,*,#2732,.T.);
#3533=ORIENTED_EDGE('',*,*,#2729,.T.);
#3534=ORIENTED_EDGE('',*,*,#2711,.T.);
#3535=ORIENTED_EDGE('',*,*,#2714,.T.);
#3536=ORIENTED_EDGE('',*,*,#2717,.T.);
#3537=ORIENTED_EDGE('',*,*,#2720,.T.);
#3538=ORIENTED_EDGE('',*,*,#2737,.F.);
#3539=ORIENTED_EDGE('',*,*,#2727,.F.);
#3540=ORIENTED_EDGE('',*,*,#2731,.F.);
#3541=ORIENTED_EDGE('',*,*,#2734,.F.);
#3542=ORIENTED_EDGE('',*,*,#2739,.F.);
#3543=ORIENTED_EDGE('',*,*,#2740,.T.);
#3544=ORIENTED_EDGE('',*,*,#2741,.T.);
#3545=ORIENTED_EDGE('',*,*,#2740,.F.);
#3546=ORIENTED_EDGE('',*,*,#2742,.F.);
#3547=ORIENTED_EDGE('',*,*,#2743,.T.);
#3548=ORIENTED_EDGE('',*,*,#2744,.T.);
#3549=ORIENTED_EDGE('',*,*,#2743,.F.);
#3550=ORIENTED_EDGE('',*,*,#2742,.T.);
#3551=ORIENTED_EDGE('',*,*,#2739,.T.);
#3552=ORIENTED_EDGE('',*,*,#2744,.F.);
#3553=ORIENTED_EDGE('',*,*,#2741,.F.);
#3554=ORIENTED_EDGE('',*,*,#2745,.F.);
#3555=ORIENTED_EDGE('',*,*,#2746,.T.);
#3556=ORIENTED_EDGE('',*,*,#2747,.T.);
#3557=ORIENTED_EDGE('',*,*,#2746,.F.);
#3558=ORIENTED_EDGE('',*,*,#2748,.F.);
#3559=ORIENTED_EDGE('',*,*,#2749,.T.);
#3560=ORIENTED_EDGE('',*,*,#2750,.T.);
#3561=ORIENTED_EDGE('',*,*,#2749,.F.);
#3562=ORIENTED_EDGE('',*,*,#2748,.T.);
#3563=ORIENTED_EDGE('',*,*,#2745,.T.);
#3564=ORIENTED_EDGE('',*,*,#2750,.F.);
#3565=ORIENTED_EDGE('',*,*,#2747,.F.);
#3566=ORIENTED_EDGE('',*,*,#2751,.F.);
#3567=ORIENTED_EDGE('',*,*,#2752,.T.);
#3568=ORIENTED_EDGE('',*,*,#2753,.F.);
#3569=ORIENTED_EDGE('',*,*,#2752,.F.);
#3570=ORIENTED_EDGE('',*,*,#2754,.F.);
#3571=ORIENTED_EDGE('',*,*,#2755,.T.);
#3572=ORIENTED_EDGE('',*,*,#2756,.F.);
#3573=ORIENTED_EDGE('',*,*,#2755,.F.);
#3574=ORIENTED_EDGE('',*,*,#2757,.F.);
#3575=ORIENTED_EDGE('',*,*,#2758,.T.);
#3576=ORIENTED_EDGE('',*,*,#2759,.F.);
#3577=ORIENTED_EDGE('',*,*,#2758,.F.);
#3578=ORIENTED_EDGE('',*,*,#2760,.F.);
#3579=ORIENTED_EDGE('',*,*,#2761,.T.);
#3580=ORIENTED_EDGE('',*,*,#2762,.F.);
#3581=ORIENTED_EDGE('',*,*,#2761,.F.);
#3582=ORIENTED_EDGE('',*,*,#2763,.F.);
#3583=ORIENTED_EDGE('',*,*,#2764,.T.);
#3584=ORIENTED_EDGE('',*,*,#2765,.F.);
#3585=ORIENTED_EDGE('',*,*,#2764,.F.);
#3586=ORIENTED_EDGE('',*,*,#2766,.F.);
#3587=ORIENTED_EDGE('',*,*,#2767,.T.);
#3588=ORIENTED_EDGE('',*,*,#2768,.F.);
#3589=ORIENTED_EDGE('',*,*,#2767,.F.);
#3590=ORIENTED_EDGE('',*,*,#2769,.T.);
#3591=ORIENTED_EDGE('',*,*,#2770,.T.);
#3592=ORIENTED_EDGE('',*,*,#2771,.F.);
#3593=ORIENTED_EDGE('',*,*,#2772,.F.);
#3594=ORIENTED_EDGE('',*,*,#2773,.T.);
#3595=ORIENTED_EDGE('',*,*,#2772,.T.);
#3596=ORIENTED_EDGE('',*,*,#2774,.F.);
#3597=ORIENTED_EDGE('',*,*,#2775,.F.);
#3598=ORIENTED_EDGE('',*,*,#2768,.T.);
#3599=ORIENTED_EDGE('',*,*,#2765,.T.);
#3600=ORIENTED_EDGE('',*,*,#2762,.T.);
#3601=ORIENTED_EDGE('',*,*,#2759,.T.);
#3602=ORIENTED_EDGE('',*,*,#2756,.T.);
#3603=ORIENTED_EDGE('',*,*,#2753,.T.);
#3604=ORIENTED_EDGE('',*,*,#2776,.T.);
#3605=ORIENTED_EDGE('',*,*,#2775,.T.);
#3606=ORIENTED_EDGE('',*,*,#2777,.F.);
#3607=ORIENTED_EDGE('',*,*,#2778,.F.);
#3608=ORIENTED_EDGE('',*,*,#2779,.T.);
#3609=ORIENTED_EDGE('',*,*,#2778,.T.);
#3610=ORIENTED_EDGE('',*,*,#2780,.F.);
#3611=ORIENTED_EDGE('',*,*,#2770,.F.);
#3612=ORIENTED_EDGE('',*,*,#2766,.T.);
#3613=ORIENTED_EDGE('',*,*,#2763,.T.);
#3614=ORIENTED_EDGE('',*,*,#2760,.T.);
#3615=ORIENTED_EDGE('',*,*,#2757,.T.);
#3616=ORIENTED_EDGE('',*,*,#2754,.T.);
#3617=ORIENTED_EDGE('',*,*,#2751,.T.);
#3618=ORIENTED_EDGE('',*,*,#2780,.T.);
#3619=ORIENTED_EDGE('',*,*,#2777,.T.);
#3620=ORIENTED_EDGE('',*,*,#2774,.T.);
#3621=ORIENTED_EDGE('',*,*,#2771,.T.);
#3622=ORIENTED_EDGE('',*,*,#2779,.F.);
#3623=ORIENTED_EDGE('',*,*,#2769,.F.);
#3624=ORIENTED_EDGE('',*,*,#2773,.F.);
#3625=ORIENTED_EDGE('',*,*,#2776,.F.);
#3626=ORIENTED_EDGE('',*,*,#2781,.F.);
#3627=ORIENTED_EDGE('',*,*,#2782,.T.);
#3628=ORIENTED_EDGE('',*,*,#2783,.F.);
#3629=ORIENTED_EDGE('',*,*,#2782,.F.);
#3630=ORIENTED_EDGE('',*,*,#2784,.F.);
#3631=ORIENTED_EDGE('',*,*,#2785,.T.);
#3632=ORIENTED_EDGE('',*,*,#2786,.F.);
#3633=ORIENTED_EDGE('',*,*,#2785,.F.);
#3634=ORIENTED_EDGE('',*,*,#2787,.F.);
#3635=ORIENTED_EDGE('',*,*,#2788,.T.);
#3636=ORIENTED_EDGE('',*,*,#2789,.F.);
#3637=ORIENTED_EDGE('',*,*,#2788,.F.);
#3638=ORIENTED_EDGE('',*,*,#2790,.F.);
#3639=ORIENTED_EDGE('',*,*,#2791,.T.);
#3640=ORIENTED_EDGE('',*,*,#2792,.F.);
#3641=ORIENTED_EDGE('',*,*,#2791,.F.);
#3642=ORIENTED_EDGE('',*,*,#2793,.F.);
#3643=ORIENTED_EDGE('',*,*,#2794,.T.);
#3644=ORIENTED_EDGE('',*,*,#2795,.F.);
#3645=ORIENTED_EDGE('',*,*,#2794,.F.);
#3646=ORIENTED_EDGE('',*,*,#2796,.F.);
#3647=ORIENTED_EDGE('',*,*,#2797,.T.);
#3648=ORIENTED_EDGE('',*,*,#2798,.F.);
#3649=ORIENTED_EDGE('',*,*,#2797,.F.);
#3650=ORIENTED_EDGE('',*,*,#2799,.T.);
#3651=ORIENTED_EDGE('',*,*,#2800,.T.);
#3652=ORIENTED_EDGE('',*,*,#2801,.F.);
#3653=ORIENTED_EDGE('',*,*,#2802,.F.);
#3654=ORIENTED_EDGE('',*,*,#2803,.T.);
#3655=ORIENTED_EDGE('',*,*,#2802,.T.);
#3656=ORIENTED_EDGE('',*,*,#2804,.F.);
#3657=ORIENTED_EDGE('',*,*,#2805,.F.);
#3658=ORIENTED_EDGE('',*,*,#2798,.T.);
#3659=ORIENTED_EDGE('',*,*,#2795,.T.);
#3660=ORIENTED_EDGE('',*,*,#2792,.T.);
#3661=ORIENTED_EDGE('',*,*,#2789,.T.);
#3662=ORIENTED_EDGE('',*,*,#2786,.T.);
#3663=ORIENTED_EDGE('',*,*,#2783,.T.);
#3664=ORIENTED_EDGE('',*,*,#2806,.T.);
#3665=ORIENTED_EDGE('',*,*,#2805,.T.);
#3666=ORIENTED_EDGE('',*,*,#2807,.F.);
#3667=ORIENTED_EDGE('',*,*,#2808,.F.);
#3668=ORIENTED_EDGE('',*,*,#2809,.T.);
#3669=ORIENTED_EDGE('',*,*,#2808,.T.);
#3670=ORIENTED_EDGE('',*,*,#2810,.F.);
#3671=ORIENTED_EDGE('',*,*,#2800,.F.);
#3672=ORIENTED_EDGE('',*,*,#2796,.T.);
#3673=ORIENTED_EDGE('',*,*,#2793,.T.);
#3674=ORIENTED_EDGE('',*,*,#2790,.T.);
#3675=ORIENTED_EDGE('',*,*,#2787,.T.);
#3676=ORIENTED_EDGE('',*,*,#2784,.T.);
#3677=ORIENTED_EDGE('',*,*,#2781,.T.);
#3678=ORIENTED_EDGE('',*,*,#2810,.T.);
#3679=ORIENTED_EDGE('',*,*,#2807,.T.);
#3680=ORIENTED_EDGE('',*,*,#2804,.T.);
#3681=ORIENTED_EDGE('',*,*,#2801,.T.);
#3682=ORIENTED_EDGE('',*,*,#2809,.F.);
#3683=ORIENTED_EDGE('',*,*,#2799,.F.);
#3684=ORIENTED_EDGE('',*,*,#2803,.F.);
#3685=ORIENTED_EDGE('',*,*,#2806,.F.);
#3686=ORIENTED_EDGE('',*,*,#2811,.F.);
#3687=ORIENTED_EDGE('',*,*,#2812,.T.);
#3688=ORIENTED_EDGE('',*,*,#2813,.F.);
#3689=ORIENTED_EDGE('',*,*,#2812,.F.);
#3690=ORIENTED_EDGE('',*,*,#2814,.F.);
#3691=ORIENTED_EDGE('',*,*,#2815,.T.);
#3692=ORIENTED_EDGE('',*,*,#2816,.F.);
#3693=ORIENTED_EDGE('',*,*,#2815,.F.);
#3694=ORIENTED_EDGE('',*,*,#2817,.F.);
#3695=ORIENTED_EDGE('',*,*,#2818,.T.);
#3696=ORIENTED_EDGE('',*,*,#2819,.F.);
#3697=ORIENTED_EDGE('',*,*,#2818,.F.);
#3698=ORIENTED_EDGE('',*,*,#2820,.F.);
#3699=ORIENTED_EDGE('',*,*,#2821,.T.);
#3700=ORIENTED_EDGE('',*,*,#2822,.F.);
#3701=ORIENTED_EDGE('',*,*,#2821,.F.);
#3702=ORIENTED_EDGE('',*,*,#2823,.F.);
#3703=ORIENTED_EDGE('',*,*,#2824,.T.);
#3704=ORIENTED_EDGE('',*,*,#2825,.F.);
#3705=ORIENTED_EDGE('',*,*,#2824,.F.);
#3706=ORIENTED_EDGE('',*,*,#2826,.T.);
#3707=ORIENTED_EDGE('',*,*,#2827,.T.);
#3708=ORIENTED_EDGE('',*,*,#2828,.F.);
#3709=ORIENTED_EDGE('',*,*,#2829,.F.);
#3710=ORIENTED_EDGE('',*,*,#2830,.T.);
#3711=ORIENTED_EDGE('',*,*,#2829,.T.);
#3712=ORIENTED_EDGE('',*,*,#2831,.F.);
#3713=ORIENTED_EDGE('',*,*,#2832,.F.);
#3714=ORIENTED_EDGE('',*,*,#2833,.T.);
#3715=ORIENTED_EDGE('',*,*,#2832,.T.);
#3716=ORIENTED_EDGE('',*,*,#2834,.F.);
#3717=ORIENTED_EDGE('',*,*,#2835,.F.);
#3718=ORIENTED_EDGE('',*,*,#2836,.T.);
#3719=ORIENTED_EDGE('',*,*,#2835,.T.);
#3720=ORIENTED_EDGE('',*,*,#2837,.F.);
#3721=ORIENTED_EDGE('',*,*,#2827,.F.);
#3722=ORIENTED_EDGE('',*,*,#2837,.T.);
#3723=ORIENTED_EDGE('',*,*,#2834,.T.);
#3724=ORIENTED_EDGE('',*,*,#2831,.T.);
#3725=ORIENTED_EDGE('',*,*,#2828,.T.);
#3726=ORIENTED_EDGE('',*,*,#2813,.T.);
#3727=ORIENTED_EDGE('',*,*,#2816,.T.);
#3728=ORIENTED_EDGE('',*,*,#2819,.T.);
#3729=ORIENTED_EDGE('',*,*,#2822,.T.);
#3730=ORIENTED_EDGE('',*,*,#2825,.T.);
#3731=ORIENTED_EDGE('',*,*,#2836,.F.);
#3732=ORIENTED_EDGE('',*,*,#2826,.F.);
#3733=ORIENTED_EDGE('',*,*,#2830,.F.);
#3734=ORIENTED_EDGE('',*,*,#2833,.F.);
#3735=ORIENTED_EDGE('',*,*,#2811,.T.);
#3736=ORIENTED_EDGE('',*,*,#2814,.T.);
#3737=ORIENTED_EDGE('',*,*,#2817,.T.);
#3738=ORIENTED_EDGE('',*,*,#2820,.T.);
#3739=ORIENTED_EDGE('',*,*,#2823,.T.);
#3740=ORIENTED_EDGE('',*,*,#2838,.F.);
#3741=ORIENTED_EDGE('',*,*,#2839,.T.);
#3742=ORIENTED_EDGE('',*,*,#2840,.T.);
#3743=ORIENTED_EDGE('',*,*,#2839,.F.);
#3744=ORIENTED_EDGE('',*,*,#2841,.F.);
#3745=ORIENTED_EDGE('',*,*,#2842,.T.);
#3746=ORIENTED_EDGE('',*,*,#2843,.T.);
#3747=ORIENTED_EDGE('',*,*,#2842,.F.);
#3748=ORIENTED_EDGE('',*,*,#2841,.T.);
#3749=ORIENTED_EDGE('',*,*,#2838,.T.);
#3750=ORIENTED_EDGE('',*,*,#2843,.F.);
#3751=ORIENTED_EDGE('',*,*,#2840,.F.);
#3752=ORIENTED_EDGE('',*,*,#2844,.F.);
#3753=ORIENTED_EDGE('',*,*,#2845,.F.);
#3754=ORIENTED_EDGE('',*,*,#2846,.F.);
#3755=ORIENTED_EDGE('',*,*,#2847,.F.);
#3756=ORIENTED_EDGE('',*,*,#2848,.F.);
#3757=ORIENTED_EDGE('',*,*,#2847,.T.);
#3758=ORIENTED_EDGE('',*,*,#2849,.F.);
#3759=ORIENTED_EDGE('',*,*,#2850,.T.);
#3760=ORIENTED_EDGE('',*,*,#2851,.F.);
#3761=ORIENTED_EDGE('',*,*,#2850,.F.);
#3762=ORIENTED_EDGE('',*,*,#2852,.F.);
#3763=ORIENTED_EDGE('',*,*,#2853,.F.);
#3764=ORIENTED_EDGE('',*,*,#2854,.F.);
#3765=ORIENTED_EDGE('',*,*,#2853,.T.);
#3766=ORIENTED_EDGE('',*,*,#2855,.T.);
#3767=ORIENTED_EDGE('',*,*,#2845,.T.);
#3768=ORIENTED_EDGE('',*,*,#2855,.F.);
#3769=ORIENTED_EDGE('',*,*,#2852,.T.);
#3770=ORIENTED_EDGE('',*,*,#2849,.T.);
#3771=ORIENTED_EDGE('',*,*,#2846,.T.);
#3772=ORIENTED_EDGE('',*,*,#2856,.F.);
#3773=ORIENTED_EDGE('',*,*,#2857,.T.);
#3774=ORIENTED_EDGE('',*,*,#2858,.F.);
#3775=ORIENTED_EDGE('',*,*,#2859,.T.);
#3776=ORIENTED_EDGE('',*,*,#2856,.T.);
#3777=ORIENTED_EDGE('',*,*,#2859,.F.);
#3778=ORIENTED_EDGE('',*,*,#2858,.T.);
#3779=ORIENTED_EDGE('',*,*,#2860,.F.);
#3780=ORIENTED_EDGE('',*,*,#2861,.F.);
#3781=ORIENTED_EDGE('',*,*,#2862,.T.);
#3782=ORIENTED_EDGE('',*,*,#2860,.T.);
#3783=ORIENTED_EDGE('',*,*,#2862,.F.);
#3784=ORIENTED_EDGE('',*,*,#2863,.F.);
#3785=ORIENTED_EDGE('',*,*,#2861,.T.);
#3786=ORIENTED_EDGE('',*,*,#2864,.F.);
#3787=ORIENTED_EDGE('',*,*,#2865,.T.);
#3788=ORIENTED_EDGE('',*,*,#2863,.T.);
#3789=ORIENTED_EDGE('',*,*,#2865,.F.);
#3790=ORIENTED_EDGE('',*,*,#2864,.T.);
#3791=ORIENTED_EDGE('',*,*,#2866,.F.);
#3792=ORIENTED_EDGE('',*,*,#2867,.F.);
#3793=ORIENTED_EDGE('',*,*,#2868,.T.);
#3794=ORIENTED_EDGE('',*,*,#2866,.T.);
#3795=ORIENTED_EDGE('',*,*,#2868,.F.);
#3796=ORIENTED_EDGE('',*,*,#2869,.F.);
#3797=ORIENTED_EDGE('',*,*,#2867,.T.);
#3798=ORIENTED_EDGE('',*,*,#2870,.F.);
#3799=ORIENTED_EDGE('',*,*,#2871,.T.);
#3800=ORIENTED_EDGE('',*,*,#2869,.T.);
#3801=ORIENTED_EDGE('',*,*,#2871,.F.);
#3802=ORIENTED_EDGE('',*,*,#2870,.T.);
#3803=ORIENTED_EDGE('',*,*,#2872,.F.);
#3804=ORIENTED_EDGE('',*,*,#2872,.T.);
#3805=ORIENTED_EDGE('',*,*,#2873,.T.);
#3806=ORIENTED_EDGE('',*,*,#2857,.F.);
#3807=ORIENTED_EDGE('',*,*,#2873,.F.);
#3808=ORIENTED_EDGE('',*,*,#2851,.T.);
#3809=ORIENTED_EDGE('',*,*,#2854,.T.);
#3810=ORIENTED_EDGE('',*,*,#2844,.T.);
#3811=ORIENTED_EDGE('',*,*,#2848,.T.);
#3812=ORIENTED_EDGE('',*,*,#2874,.F.);
#3813=ORIENTED_EDGE('',*,*,#2875,.F.);
#3814=ORIENTED_EDGE('',*,*,#2876,.F.);
#3815=ORIENTED_EDGE('',*,*,#2877,.F.);
#3816=ORIENTED_EDGE('',*,*,#2878,.F.);
#3817=ORIENTED_EDGE('',*,*,#2877,.T.);
#3818=ORIENTED_EDGE('',*,*,#2879,.F.);
#3819=ORIENTED_EDGE('',*,*,#2880,.T.);
#3820=ORIENTED_EDGE('',*,*,#2881,.F.);
#3821=ORIENTED_EDGE('',*,*,#2880,.F.);
#3822=ORIENTED_EDGE('',*,*,#2882,.F.);
#3823=ORIENTED_EDGE('',*,*,#2883,.F.);
#3824=ORIENTED_EDGE('',*,*,#2884,.F.);
#3825=ORIENTED_EDGE('',*,*,#2883,.T.);
#3826=ORIENTED_EDGE('',*,*,#2885,.F.);
#3827=ORIENTED_EDGE('',*,*,#2875,.T.);
#3828=ORIENTED_EDGE('',*,*,#2886,.F.);
#3829=ORIENTED_EDGE('',*,*,#2887,.T.);
#3830=ORIENTED_EDGE('',*,*,#2888,.F.);
#3831=ORIENTED_EDGE('',*,*,#2889,.T.);
#3832=ORIENTED_EDGE('',*,*,#2886,.T.);
#3833=ORIENTED_EDGE('',*,*,#2889,.F.);
#3834=ORIENTED_EDGE('',*,*,#2881,.T.);
#3835=ORIENTED_EDGE('',*,*,#2884,.T.);
#3836=ORIENTED_EDGE('',*,*,#2874,.T.);
#3837=ORIENTED_EDGE('',*,*,#2878,.T.);
#3838=ORIENTED_EDGE('',*,*,#2888,.T.);
#3839=ORIENTED_EDGE('',*,*,#2890,.F.);
#3840=ORIENTED_EDGE('',*,*,#2890,.T.);
#3841=ORIENTED_EDGE('',*,*,#2891,.T.);
#3842=ORIENTED_EDGE('',*,*,#2887,.F.);
#3843=ORIENTED_EDGE('',*,*,#2891,.F.);
#3844=ORIENTED_EDGE('',*,*,#2882,.T.);
#3845=ORIENTED_EDGE('',*,*,#2879,.T.);
#3846=ORIENTED_EDGE('',*,*,#2876,.T.);
#3847=ORIENTED_EDGE('',*,*,#2885,.T.);
#3848=ORIENTED_EDGE('',*,*,#2892,.F.);
#3849=ORIENTED_EDGE('',*,*,#2893,.F.);
#3850=ORIENTED_EDGE('',*,*,#2894,.T.);
#3851=ORIENTED_EDGE('',*,*,#2892,.T.);
#3852=ORIENTED_EDGE('',*,*,#2894,.F.);
#3853=ORIENTED_EDGE('',*,*,#2895,.F.);
#3854=ORIENTED_EDGE('',*,*,#2896,.T.);
#3855=ORIENTED_EDGE('',*,*,#2893,.T.);
#3856=ORIENTED_EDGE('',*,*,#2896,.F.);
#3857=ORIENTED_EDGE('',*,*,#2897,.F.);
#3858=ORIENTED_EDGE('',*,*,#2898,.T.);
#3859=ORIENTED_EDGE('',*,*,#2895,.T.);
#3860=ORIENTED_EDGE('',*,*,#2898,.F.);
#3861=ORIENTED_EDGE('',*,*,#2897,.T.);
#3862=ORIENTED_EDGE('',*,*,#2899,.F.);
#3863=ORIENTED_EDGE('',*,*,#2900,.F.);
#3864=ORIENTED_EDGE('',*,*,#2901,.T.);
#3865=ORIENTED_EDGE('',*,*,#2899,.T.);
#3866=ORIENTED_EDGE('',*,*,#2901,.F.);
#3867=ORIENTED_EDGE('',*,*,#2902,.F.);
#3868=ORIENTED_EDGE('',*,*,#2903,.T.);
#3869=ORIENTED_EDGE('',*,*,#2900,.T.);
#3870=ORIENTED_EDGE('',*,*,#2903,.F.);
#3871=ORIENTED_EDGE('',*,*,#2904,.F.);
#3872=ORIENTED_EDGE('',*,*,#2905,.T.);
#3873=ORIENTED_EDGE('',*,*,#2902,.T.);
#3874=ORIENTED_EDGE('',*,*,#2905,.F.);
#3875=ORIENTED_EDGE('',*,*,#2904,.T.);
#3876=ORIENTED_EDGE('',*,*,#2906,.T.);
#3877=ORIENTED_EDGE('',*,*,#2907,.T.);
#3878=ORIENTED_EDGE('',*,*,#2908,.T.);
#3879=ORIENTED_EDGE('',*,*,#2909,.F.);
#3880=ORIENTED_EDGE('',*,*,#2910,.T.);
#3881=ORIENTED_EDGE('',*,*,#2911,.T.);
#3882=ORIENTED_EDGE('',*,*,#2912,.T.);
#3883=ORIENTED_EDGE('',*,*,#2907,.F.);
#3884=ORIENTED_EDGE('',*,*,#2913,.T.);
#3885=ORIENTED_EDGE('',*,*,#2914,.T.);
#3886=ORIENTED_EDGE('',*,*,#2915,.T.);
#3887=ORIENTED_EDGE('',*,*,#2911,.F.);
#3888=ORIENTED_EDGE('',*,*,#2916,.T.);
#3889=ORIENTED_EDGE('',*,*,#2917,.T.);
#3890=ORIENTED_EDGE('',*,*,#2918,.T.);
#3891=ORIENTED_EDGE('',*,*,#2914,.F.);
#3892=ORIENTED_EDGE('',*,*,#2919,.T.);
#3893=ORIENTED_EDGE('',*,*,#2920,.T.);
#3894=ORIENTED_EDGE('',*,*,#2921,.T.);
#3895=ORIENTED_EDGE('',*,*,#2917,.F.);
#3896=ORIENTED_EDGE('',*,*,#2922,.T.);
#3897=ORIENTED_EDGE('',*,*,#2909,.T.);
#3898=ORIENTED_EDGE('',*,*,#2923,.T.);
#3899=ORIENTED_EDGE('',*,*,#2920,.F.);
#3900=ORIENTED_EDGE('',*,*,#2922,.F.);
#3901=ORIENTED_EDGE('',*,*,#2919,.F.);
#3902=ORIENTED_EDGE('',*,*,#2916,.F.);
#3903=ORIENTED_EDGE('',*,*,#2913,.F.);
#3904=ORIENTED_EDGE('',*,*,#2910,.F.);
#3905=ORIENTED_EDGE('',*,*,#2906,.F.);
#3906=ORIENTED_EDGE('',*,*,#2923,.F.);
#3907=ORIENTED_EDGE('',*,*,#2908,.F.);
#3908=ORIENTED_EDGE('',*,*,#2912,.F.);
#3909=ORIENTED_EDGE('',*,*,#2915,.F.);
#3910=ORIENTED_EDGE('',*,*,#2918,.F.);
#3911=ORIENTED_EDGE('',*,*,#2921,.F.);
#3912=ORIENTED_EDGE('',*,*,#2924,.F.);
#3913=ORIENTED_EDGE('',*,*,#2925,.F.);
#3914=ORIENTED_EDGE('',*,*,#2926,.T.);
#3915=ORIENTED_EDGE('',*,*,#2924,.T.);
#3916=ORIENTED_EDGE('',*,*,#2926,.F.);
#3917=ORIENTED_EDGE('',*,*,#2927,.F.);
#3918=ORIENTED_EDGE('',*,*,#2928,.T.);
#3919=ORIENTED_EDGE('',*,*,#2925,.T.);
#3920=ORIENTED_EDGE('',*,*,#2928,.F.);
#3921=ORIENTED_EDGE('',*,*,#2929,.F.);
#3922=ORIENTED_EDGE('',*,*,#2930,.T.);
#3923=ORIENTED_EDGE('',*,*,#2927,.T.);
#3924=ORIENTED_EDGE('',*,*,#2930,.F.);
#3925=ORIENTED_EDGE('',*,*,#2929,.T.);
#3926=ORIENTED_EDGE('',*,*,#2931,.F.);
#3927=ORIENTED_EDGE('',*,*,#2932,.F.);
#3928=ORIENTED_EDGE('',*,*,#2933,.T.);
#3929=ORIENTED_EDGE('',*,*,#2931,.T.);
#3930=ORIENTED_EDGE('',*,*,#2933,.F.);
#3931=ORIENTED_EDGE('',*,*,#2934,.F.);
#3932=ORIENTED_EDGE('',*,*,#2935,.T.);
#3933=ORIENTED_EDGE('',*,*,#2932,.T.);
#3934=ORIENTED_EDGE('',*,*,#2935,.F.);
#3935=ORIENTED_EDGE('',*,*,#2936,.F.);
#3936=ORIENTED_EDGE('',*,*,#2937,.T.);
#3937=ORIENTED_EDGE('',*,*,#2934,.T.);
#3938=ORIENTED_EDGE('',*,*,#2937,.F.);
#3939=ORIENTED_EDGE('',*,*,#2936,.T.);
#3940=ORIENTED_EDGE('',*,*,#2938,.T.);
#3941=ORIENTED_EDGE('',*,*,#2939,.T.);
#3942=ORIENTED_EDGE('',*,*,#2940,.T.);
#3943=ORIENTED_EDGE('',*,*,#2941,.F.);
#3944=ORIENTED_EDGE('',*,*,#2942,.T.);
#3945=ORIENTED_EDGE('',*,*,#2943,.T.);
#3946=ORIENTED_EDGE('',*,*,#2944,.T.);
#3947=ORIENTED_EDGE('',*,*,#2939,.F.);
#3948=ORIENTED_EDGE('',*,*,#2945,.T.);
#3949=ORIENTED_EDGE('',*,*,#2946,.T.);
#3950=ORIENTED_EDGE('',*,*,#2947,.T.);
#3951=ORIENTED_EDGE('',*,*,#2943,.F.);
#3952=ORIENTED_EDGE('',*,*,#2948,.T.);
#3953=ORIENTED_EDGE('',*,*,#2949,.T.);
#3954=ORIENTED_EDGE('',*,*,#2950,.T.);
#3955=ORIENTED_EDGE('',*,*,#2946,.F.);
#3956=ORIENTED_EDGE('',*,*,#2951,.T.);
#3957=ORIENTED_EDGE('',*,*,#2952,.T.);
#3958=ORIENTED_EDGE('',*,*,#2953,.T.);
#3959=ORIENTED_EDGE('',*,*,#2949,.F.);
#3960=ORIENTED_EDGE('',*,*,#2954,.T.);
#3961=ORIENTED_EDGE('',*,*,#2941,.T.);
#3962=ORIENTED_EDGE('',*,*,#2955,.T.);
#3963=ORIENTED_EDGE('',*,*,#2952,.F.);
#3964=ORIENTED_EDGE('',*,*,#2954,.F.);
#3965=ORIENTED_EDGE('',*,*,#2951,.F.);
#3966=ORIENTED_EDGE('',*,*,#2948,.F.);
#3967=ORIENTED_EDGE('',*,*,#2945,.F.);
#3968=ORIENTED_EDGE('',*,*,#2942,.F.);
#3969=ORIENTED_EDGE('',*,*,#2938,.F.);
#3970=ORIENTED_EDGE('',*,*,#2955,.F.);
#3971=ORIENTED_EDGE('',*,*,#2940,.F.);
#3972=ORIENTED_EDGE('',*,*,#2944,.F.);
#3973=ORIENTED_EDGE('',*,*,#2947,.F.);
#3974=ORIENTED_EDGE('',*,*,#2950,.F.);
#3975=ORIENTED_EDGE('',*,*,#2953,.F.);
#3976=ORIENTED_EDGE('',*,*,#2956,.F.);
#3977=ORIENTED_EDGE('',*,*,#2957,.T.);
#3978=ORIENTED_EDGE('',*,*,#2958,.T.);
#3979=ORIENTED_EDGE('',*,*,#2957,.F.);
#3980=ORIENTED_EDGE('',*,*,#2959,.F.);
#3981=ORIENTED_EDGE('',*,*,#2960,.T.);
#3982=ORIENTED_EDGE('',*,*,#2961,.T.);
#3983=ORIENTED_EDGE('',*,*,#2960,.F.);
#3984=ORIENTED_EDGE('',*,*,#2959,.T.);
#3985=ORIENTED_EDGE('',*,*,#2956,.T.);
#3986=ORIENTED_EDGE('',*,*,#2961,.F.);
#3987=ORIENTED_EDGE('',*,*,#2958,.F.);
#3988=ORIENTED_EDGE('',*,*,#2962,.F.);
#3989=ORIENTED_EDGE('',*,*,#2963,.F.);
#3990=ORIENTED_EDGE('',*,*,#2964,.T.);
#3991=ORIENTED_EDGE('',*,*,#2962,.T.);
#3992=ORIENTED_EDGE('',*,*,#2964,.F.);
#3993=ORIENTED_EDGE('',*,*,#2965,.F.);
#3994=ORIENTED_EDGE('',*,*,#2966,.T.);
#3995=ORIENTED_EDGE('',*,*,#2963,.T.);
#3996=ORIENTED_EDGE('',*,*,#2966,.F.);
#3997=ORIENTED_EDGE('',*,*,#2967,.F.);
#3998=ORIENTED_EDGE('',*,*,#2968,.T.);
#3999=ORIENTED_EDGE('',*,*,#2965,.T.);
#4000=ORIENTED_EDGE('',*,*,#2968,.F.);
#4001=ORIENTED_EDGE('',*,*,#2967,.T.);
#4002=ORIENTED_EDGE('',*,*,#2969,.F.);
#4003=ORIENTED_EDGE('',*,*,#2970,.F.);
#4004=ORIENTED_EDGE('',*,*,#2971,.T.);
#4005=ORIENTED_EDGE('',*,*,#2969,.T.);
#4006=ORIENTED_EDGE('',*,*,#2971,.F.);
#4007=ORIENTED_EDGE('',*,*,#2972,.F.);
#4008=ORIENTED_EDGE('',*,*,#2973,.T.);
#4009=ORIENTED_EDGE('',*,*,#2970,.T.);
#4010=ORIENTED_EDGE('',*,*,#2973,.F.);
#4011=ORIENTED_EDGE('',*,*,#2974,.F.);
#4012=ORIENTED_EDGE('',*,*,#2975,.T.);
#4013=ORIENTED_EDGE('',*,*,#2972,.T.);
#4014=ORIENTED_EDGE('',*,*,#2975,.F.);
#4015=ORIENTED_EDGE('',*,*,#2974,.T.);
#4016=ORIENTED_EDGE('',*,*,#2976,.T.);
#4017=ORIENTED_EDGE('',*,*,#2977,.T.);
#4018=ORIENTED_EDGE('',*,*,#2978,.T.);
#4019=ORIENTED_EDGE('',*,*,#2979,.F.);
#4020=ORIENTED_EDGE('',*,*,#2980,.T.);
#4021=ORIENTED_EDGE('',*,*,#2981,.T.);
#4022=ORIENTED_EDGE('',*,*,#2982,.T.);
#4023=ORIENTED_EDGE('',*,*,#2977,.F.);
#4024=ORIENTED_EDGE('',*,*,#2983,.T.);
#4025=ORIENTED_EDGE('',*,*,#2984,.T.);
#4026=ORIENTED_EDGE('',*,*,#2985,.T.);
#4027=ORIENTED_EDGE('',*,*,#2981,.F.);
#4028=ORIENTED_EDGE('',*,*,#2986,.T.);
#4029=ORIENTED_EDGE('',*,*,#2987,.T.);
#4030=ORIENTED_EDGE('',*,*,#2988,.T.);
#4031=ORIENTED_EDGE('',*,*,#2984,.F.);
#4032=ORIENTED_EDGE('',*,*,#2989,.T.);
#4033=ORIENTED_EDGE('',*,*,#2990,.T.);
#4034=ORIENTED_EDGE('',*,*,#2991,.T.);
#4035=ORIENTED_EDGE('',*,*,#2987,.F.);
#4036=ORIENTED_EDGE('',*,*,#2992,.T.);
#4037=ORIENTED_EDGE('',*,*,#2979,.T.);
#4038=ORIENTED_EDGE('',*,*,#2993,.T.);
#4039=ORIENTED_EDGE('',*,*,#2990,.F.);
#4040=ORIENTED_EDGE('',*,*,#2992,.F.);
#4041=ORIENTED_EDGE('',*,*,#2989,.F.);
#4042=ORIENTED_EDGE('',*,*,#2986,.F.);
#4043=ORIENTED_EDGE('',*,*,#2983,.F.);
#4044=ORIENTED_EDGE('',*,*,#2980,.F.);
#4045=ORIENTED_EDGE('',*,*,#2976,.F.);
#4046=ORIENTED_EDGE('',*,*,#2993,.F.);
#4047=ORIENTED_EDGE('',*,*,#2978,.F.);
#4048=ORIENTED_EDGE('',*,*,#2982,.F.);
#4049=ORIENTED_EDGE('',*,*,#2985,.F.);
#4050=ORIENTED_EDGE('',*,*,#2988,.F.);
#4051=ORIENTED_EDGE('',*,*,#2991,.F.);
#4052=CYLINDRICAL_SURFACE('',#4652,0.210000000000001);
#4053=CYLINDRICAL_SURFACE('',#4655,0.21);
#4054=CYLINDRICAL_SURFACE('',#4658,0.21);
#4055=CYLINDRICAL_SURFACE('',#4661,0.210000000000001);
#4056=CYLINDRICAL_SURFACE('',#4664,0.210000000000001);
#4057=CYLINDRICAL_SURFACE('',#4667,0.210000000000001);
#4058=CYLINDRICAL_SURFACE('',#4670,0.21);
#4059=CYLINDRICAL_SURFACE('',#4673,0.21);
#4060=CYLINDRICAL_SURFACE('',#4676,0.21);
#4061=CYLINDRICAL_SURFACE('',#4679,0.21);
#4062=CYLINDRICAL_SURFACE('',#4682,0.210000000000001);
#4063=CYLINDRICAL_SURFACE('',#4685,0.210000000000001);
#4064=CYLINDRICAL_SURFACE('',#4695,0.475);
#4065=CYLINDRICAL_SURFACE('',#4700,0.475);
#4066=CYLINDRICAL_SURFACE('',#4705,0.275);
#4067=CYLINDRICAL_SURFACE('',#4707,0.275);
#4068=CYLINDRICAL_SURFACE('',#4723,0.475000000000001);
#4069=CYLINDRICAL_SURFACE('',#4728,0.475000000000001);
#4070=CYLINDRICAL_SURFACE('',#4733,0.274999999999999);
#4071=CYLINDRICAL_SURFACE('',#4735,0.274999999999999);
#4072=CYLINDRICAL_SURFACE('',#4754,0.6);
#4073=CYLINDRICAL_SURFACE('',#4763,0.525);
#4074=CYLINDRICAL_SURFACE('',#4765,0.525);
#4075=CYLINDRICAL_SURFACE('',#4775,0.225);
#4076=CYLINDRICAL_SURFACE('',#4778,0.165);
#4077=CYLINDRICAL_SURFACE('',#4780,0.275);
#4078=CYLINDRICAL_SURFACE('',#4782,0.275);
#4079=CYLINDRICAL_SURFACE('',#4784,0.6);
#4080=CYLINDRICAL_SURFACE('',#4813,0.425);
#4081=CYLINDRICAL_SURFACE('',#4821,0.24505);
#4082=CYLINDRICAL_SURFACE('',#4824,0.165);
#4083=CYLINDRICAL_SURFACE('',#4828,0.165);
#4084=CYLINDRICAL_SURFACE('',#4832,0.165);
#4085=CYLINDRICAL_SURFACE('',#4836,0.165);
#4086=CYLINDRICAL_SURFACE('',#4840,0.165);
#4087=CYLINDRICAL_SURFACE('',#4844,0.165);
#4088=CYLINDRICAL_SURFACE('',#4848,0.165);
#4089=CYLINDRICAL_SURFACE('',#4852,0.165);
#4090=CYLINDRICAL_SURFACE('',#4856,0.210000000000001);
#4091=CYLINDRICAL_SURFACE('',#4860,0.210000000000001);
#4092=CYLINDRICAL_SURFACE('',#4864,0.210000000000001);
#4093=CYLINDRICAL_SURFACE('',#4868,0.210000000000001);
#4094=CYLINDRICAL_SURFACE('',#4872,1.05);
#4095=CYLINDRICAL_SURFACE('',#4875,1.05);
#4096=CYLINDRICAL_SURFACE('',#4885,0.7);
#4097=CYLINDRICAL_SURFACE('',#4888,1.04);
#4098=CYLINDRICAL_SURFACE('',#4894,0.7);
#4099=CYLINDRICAL_SURFACE('',#4897,1.04);
#4100=CYLINDRICAL_SURFACE('',#4903,0.225);
#4101=CYLINDRICAL_SURFACE('',#4906,0.225);
#4102=CYLINDRICAL_SURFACE('',#4909,0.225);
#4103=CYLINDRICAL_SURFACE('',#4912,0.225);
#4104=CYLINDRICAL_SURFACE('',#4915,0.7);
#4105=CYLINDRICAL_SURFACE('',#4918,0.7);
#4106=CYLINDRICAL_SURFACE('',#4928,0.225);
#4107=CYLINDRICAL_SURFACE('',#4931,0.225);
#4108=CYLINDRICAL_SURFACE('',#4934,0.225);
#4109=CYLINDRICAL_SURFACE('',#4937,0.225);
#4110=CYLINDRICAL_SURFACE('',#4940,0.7);
#4111=CYLINDRICAL_SURFACE('',#4943,0.7);
#4112=CYLINDRICAL_SURFACE('',#4953,0.25);
#4113=CYLINDRICAL_SURFACE('',#4956,0.274999999999999);
#4114=CYLINDRICAL_SURFACE('',#4959,0.275);
#4115=CYLINDRICAL_SURFACE('',#4962,0.275);
#4116=CYLINDRICAL_SURFACE('',#4965,0.274999999999999);
#4117=CYLINDRICAL_SURFACE('',#4975,0.33);
#4118=CYLINDRICAL_SURFACE('',#4978,1.5);
#4119=CYLINDRICAL_SURFACE('',#4995,1.05);
#4120=CYLINDRICAL_SURFACE('',#4999,1.);
#4121=CYLINDRICAL_SURFACE('',#5003,1.05);
#4122=CYLINDRICAL_SURFACE('',#5007,1.);
#4123=CYLINDRICAL_SURFACE('',#5011,1.05);
#4124=CYLINDRICAL_SURFACE('',#5015,0.9);
#4125=CYLINDRICAL_SURFACE('',#5028,0.895);
#4126=CYLINDRICAL_SURFACE('',#5032,0.605);
#4127=CYLINDRICAL_SURFACE('',#5040,0.35);
#4128=CYLINDRICAL_SURFACE('',#5048,0.1954);
#4129=CYLINDRICAL_SURFACE('',#5066,0.425);
#4130=CYLINDRICAL_SURFACE('',#5074,0.24505);
#4131=CYLINDRICAL_SURFACE('',#5115,0.32);
#4132=CYLINDRICAL_SURFACE('',#5118,0.6);
#4133=CYLINDRICAL_SURFACE('',#5128,0.5);
#4134=CYLINDRICAL_SURFACE('',#5136,0.2942);
#4135=ADVANCED_FACE('',(#616),#4052,.F.);
#4136=ADVANCED_FACE('',(#617),#4053,.F.);
#4137=ADVANCED_FACE('',(#618),#4054,.F.);
#4138=ADVANCED_FACE('',(#619),#4055,.F.);
#4139=ADVANCED_FACE('',(#620),#4056,.F.);
#4140=ADVANCED_FACE('',(#621),#4057,.F.);
#4141=ADVANCED_FACE('',(#622),#4058,.F.);
#4142=ADVANCED_FACE('',(#623),#4059,.F.);
#4143=ADVANCED_FACE('',(#624),#4060,.F.);
#4144=ADVANCED_FACE('',(#625),#4061,.F.);
#4145=ADVANCED_FACE('',(#626),#4062,.F.);
#4146=ADVANCED_FACE('',(#627),#4063,.F.);
#4147=ADVANCED_FACE('',(#628),#459,.T.);
#4148=ADVANCED_FACE('',(#629),#460,.T.);
#4149=ADVANCED_FACE('',(#630),#461,.T.);
#4150=ADVANCED_FACE('',(#631),#462,.T.);
#4151=ADVANCED_FACE('',(#632,#340,#341,#342,#343,#344,#345,#346,#347,#348,
#349,#350,#351),#463,.T.);
#4152=ADVANCED_FACE('',(#633,#352,#353,#354,#355,#356,#357,#358,#359,#360,
#361,#362,#363),#464,.F.);
#4153=ADVANCED_FACE('',(#634),#4064,.F.);
#4154=ADVANCED_FACE('',(#635,#364),#465,.T.);
#4155=ADVANCED_FACE('',(#636),#4065,.F.);
#4156=ADVANCED_FACE('',(#637,#365),#466,.T.);
#4157=ADVANCED_FACE('',(#638),#4066,.F.);
#4158=ADVANCED_FACE('',(#639),#4067,.F.);
#4159=ADVANCED_FACE('',(#640),#467,.T.);
#4160=ADVANCED_FACE('',(#641),#468,.T.);
#4161=ADVANCED_FACE('',(#642),#469,.T.);
#4162=ADVANCED_FACE('',(#643),#470,.T.);
#4163=ADVANCED_FACE('',(#644,#366,#367),#471,.T.);
#4164=ADVANCED_FACE('',(#645,#368,#369),#472,.F.);
#4165=ADVANCED_FACE('',(#646),#473,.T.);
#4166=ADVANCED_FACE('',(#647),#474,.T.);
#4167=ADVANCED_FACE('',(#648),#475,.T.);
#4168=ADVANCED_FACE('',(#649),#476,.T.);
#4169=ADVANCED_FACE('',(#650),#477,.T.);
#4170=ADVANCED_FACE('',(#651),#478,.F.);
#4171=ADVANCED_FACE('',(#652),#4068,.F.);
#4172=ADVANCED_FACE('',(#653,#370),#479,.T.);
#4173=ADVANCED_FACE('',(#654),#4069,.F.);
#4174=ADVANCED_FACE('',(#655,#371),#480,.T.);
#4175=ADVANCED_FACE('',(#656),#4070,.F.);
#4176=ADVANCED_FACE('',(#657),#4071,.F.);
#4177=ADVANCED_FACE('',(#658),#481,.T.);
#4178=ADVANCED_FACE('',(#659),#482,.T.);
#4179=ADVANCED_FACE('',(#660),#483,.T.);
#4180=ADVANCED_FACE('',(#661),#484,.T.);
#4181=ADVANCED_FACE('',(#662,#372,#373),#485,.T.);
#4182=ADVANCED_FACE('',(#663,#374,#375),#486,.F.);
#4183=ADVANCED_FACE('',(#664),#487,.T.);
#4184=ADVANCED_FACE('',(#665),#488,.T.);
#4185=ADVANCED_FACE('',(#666),#489,.T.);
#4186=ADVANCED_FACE('',(#667),#490,.T.);
#4187=ADVANCED_FACE('',(#668),#491,.T.);
#4188=ADVANCED_FACE('',(#669),#492,.F.);
#4189=ADVANCED_FACE('',(#670),#243,.T.);
#4190=ADVANCED_FACE('',(#671),#4072,.T.);
#4191=ADVANCED_FACE('',(#672),#493,.F.);
#4192=ADVANCED_FACE('',(#673),#244,.T.);
#4193=ADVANCED_FACE('',(#674),#494,.T.);
#4194=ADVANCED_FACE('',(#675),#495,.F.);
#4195=ADVANCED_FACE('',(#676),#4073,.F.);
#4196=ADVANCED_FACE('',(#677),#4074,.F.);
#4197=ADVANCED_FACE('',(#678),#496,.F.);
#4198=ADVANCED_FACE('',(#679,#376),#497,.T.);
#4199=ADVANCED_FACE('',(#680,#377),#498,.T.);
#4200=ADVANCED_FACE('',(#681,#378),#499,.T.);
#4201=ADVANCED_FACE('',(#682),#4075,.F.);
#4202=ADVANCED_FACE('',(#683),#4076,.F.);
#4203=ADVANCED_FACE('',(#684),#4077,.F.);
#4204=ADVANCED_FACE('',(#685),#4078,.F.);
#4205=ADVANCED_FACE('',(#686),#4079,.F.);
#4206=ADVANCED_FACE('',(#687,#379),#500,.T.);
#4207=ADVANCED_FACE('',(#688),#501,.T.);
#4208=ADVANCED_FACE('',(#689,#380,#381),#502,.T.);
#4209=ADVANCED_FACE('',(#690),#503,.T.);
#4210=ADVANCED_FACE('',(#691,#382),#504,.T.);
#4211=ADVANCED_FACE('',(#692),#505,.T.);
#4212=ADVANCED_FACE('',(#693,#383),#506,.T.);
#4213=ADVANCED_FACE('',(#694),#507,.T.);
#4214=ADVANCED_FACE('',(#695,#384),#508,.T.);
#4215=ADVANCED_FACE('',(#696),#509,.T.);
#4216=ADVANCED_FACE('',(#697,#385),#510,.T.);
#4217=ADVANCED_FACE('',(#698),#511,.F.);
#4218=ADVANCED_FACE('',(#699),#512,.F.);
#4219=ADVANCED_FACE('',(#700),#513,.F.);
#4220=ADVANCED_FACE('',(#701),#514,.F.);
#4221=ADVANCED_FACE('',(#702),#515,.F.);
#4222=ADVANCED_FACE('',(#703),#516,.F.);
#4223=ADVANCED_FACE('',(#704),#517,.F.);
#4224=ADVANCED_FACE('',(#705),#518,.F.);
#4225=ADVANCED_FACE('',(#706),#519,.F.);
#4226=ADVANCED_FACE('',(#707),#520,.T.);
#4227=ADVANCED_FACE('',(#708),#245,.T.);
#4228=ADVANCED_FACE('',(#709),#4080,.T.);
#4229=ADVANCED_FACE('',(#710),#246,.T.);
#4230=ADVANCED_FACE('',(#711,#386),#521,.T.);
#4231=ADVANCED_FACE('',(#712),#247,.T.);
#4232=ADVANCED_FACE('',(#713),#4081,.T.);
#4233=ADVANCED_FACE('',(#714),#4082,.F.);
#4234=ADVANCED_FACE('',(#715),#522,.T.);
#4235=ADVANCED_FACE('',(#716),#4083,.F.);
#4236=ADVANCED_FACE('',(#717),#523,.T.);
#4237=ADVANCED_FACE('',(#718),#4084,.F.);
#4238=ADVANCED_FACE('',(#719),#524,.T.);
#4239=ADVANCED_FACE('',(#720),#4085,.F.);
#4240=ADVANCED_FACE('',(#721),#525,.T.);
#4241=ADVANCED_FACE('',(#722),#4086,.F.);
#4242=ADVANCED_FACE('',(#723),#526,.F.);
#4243=ADVANCED_FACE('',(#724),#4087,.F.);
#4244=ADVANCED_FACE('',(#725),#527,.F.);
#4245=ADVANCED_FACE('',(#726),#4088,.F.);
#4246=ADVANCED_FACE('',(#727),#528,.F.);
#4247=ADVANCED_FACE('',(#728),#4089,.F.);
#4248=ADVANCED_FACE('',(#729),#529,.F.);
#4249=ADVANCED_FACE('',(#730),#4090,.F.);
#4250=ADVANCED_FACE('',(#731),#530,.T.);
#4251=ADVANCED_FACE('',(#732),#4091,.F.);
#4252=ADVANCED_FACE('',(#733),#531,.T.);
#4253=ADVANCED_FACE('',(#734),#4092,.F.);
#4254=ADVANCED_FACE('',(#735),#532,.T.);
#4255=ADVANCED_FACE('',(#736),#4093,.F.);
#4256=ADVANCED_FACE('',(#737),#533,.T.);
#4257=ADVANCED_FACE('',(#738),#4094,.F.);
#4258=ADVANCED_FACE('',(#739),#4095,.F.);
#4259=ADVANCED_FACE('',(#740),#534,.T.);
#4260=ADVANCED_FACE('',(#741,#387,#388,#389,#390,#391,#392),#535,.T.);
#4261=ADVANCED_FACE('',(#742),#536,.T.);
#4262=ADVANCED_FACE('',(#743,#393,#394,#395,#396,#397,#398),#537,.T.);
#4263=ADVANCED_FACE('',(#744,#399,#400,#401,#402),#538,.T.);
#4264=ADVANCED_FACE('',(#745),#539,.F.);
#4265=ADVANCED_FACE('',(#746),#4096,.F.);
#4266=ADVANCED_FACE('',(#747),#4097,.T.);
#4267=ADVANCED_FACE('',(#748,#403),#540,.T.);
#4268=ADVANCED_FACE('',(#749,#404),#541,.F.);
#4269=ADVANCED_FACE('',(#750),#4098,.F.);
#4270=ADVANCED_FACE('',(#751),#4099,.T.);
#4271=ADVANCED_FACE('',(#752,#405),#542,.T.);
#4272=ADVANCED_FACE('',(#753,#406),#543,.F.);
#4273=ADVANCED_FACE('',(#754),#4100,.F.);
#4274=ADVANCED_FACE('',(#755),#4101,.F.);
#4275=ADVANCED_FACE('',(#756),#4102,.F.);
#4276=ADVANCED_FACE('',(#757),#4103,.F.);
#4277=ADVANCED_FACE('',(#758),#4104,.F.);
#4278=ADVANCED_FACE('',(#759),#4105,.F.);
#4279=ADVANCED_FACE('',(#760),#544,.T.);
#4280=ADVANCED_FACE('',(#761,#407,#408,#409,#410,#411,#412),#545,.T.);
#4281=ADVANCED_FACE('',(#762),#546,.T.);
#4282=ADVANCED_FACE('',(#763,#413,#414,#415,#416,#417,#418),#547,.T.);
#4283=ADVANCED_FACE('',(#764),#548,.T.);
#4284=ADVANCED_FACE('',(#765),#549,.F.);
#4285=ADVANCED_FACE('',(#766),#4106,.F.);
#4286=ADVANCED_FACE('',(#767),#4107,.F.);
#4287=ADVANCED_FACE('',(#768),#4108,.F.);
#4288=ADVANCED_FACE('',(#769),#4109,.F.);
#4289=ADVANCED_FACE('',(#770),#4110,.F.);
#4290=ADVANCED_FACE('',(#771),#4111,.F.);
#4291=ADVANCED_FACE('',(#772),#550,.T.);
#4292=ADVANCED_FACE('',(#773,#419,#420,#421,#422,#423,#424),#551,.T.);
#4293=ADVANCED_FACE('',(#774),#552,.T.);
#4294=ADVANCED_FACE('',(#775,#425,#426,#427,#428,#429,#430),#553,.T.);
#4295=ADVANCED_FACE('',(#776),#554,.T.);
#4296=ADVANCED_FACE('',(#777),#555,.F.);
#4297=ADVANCED_FACE('',(#778),#4112,.F.);
#4298=ADVANCED_FACE('',(#779),#4113,.F.);
#4299=ADVANCED_FACE('',(#780),#4114,.F.);
#4300=ADVANCED_FACE('',(#781),#4115,.F.);
#4301=ADVANCED_FACE('',(#782),#4116,.F.);
#4302=ADVANCED_FACE('',(#783),#556,.T.);
#4303=ADVANCED_FACE('',(#784),#557,.T.);
#4304=ADVANCED_FACE('',(#785),#558,.T.);
#4305=ADVANCED_FACE('',(#786),#559,.T.);
#4306=ADVANCED_FACE('',(#787,#431,#432,#433,#434,#435),#560,.T.);
#4307=ADVANCED_FACE('',(#788,#436,#437,#438,#439,#440),#561,.F.);
#4308=ADVANCED_FACE('',(#789),#4117,.F.);
#4309=ADVANCED_FACE('',(#790),#4118,.T.);
#4310=ADVANCED_FACE('',(#791,#441),#562,.T.);
#4311=ADVANCED_FACE('',(#792,#442),#563,.F.);
#4312=ADVANCED_FACE('',(#793),#564,.F.);
#4313=ADVANCED_FACE('',(#794),#565,.F.);
#4314=ADVANCED_FACE('',(#795),#566,.F.);
#4315=ADVANCED_FACE('',(#796),#567,.F.);
#4316=ADVANCED_FACE('',(#797),#568,.F.);
#4317=ADVANCED_FACE('',(#798,#443),#569,.T.);
#4318=ADVANCED_FACE('',(#799),#4119,.T.);
#4319=ADVANCED_FACE('',(#800,#444),#570,.T.);
#4320=ADVANCED_FACE('',(#801),#4120,.T.);
#4321=ADVANCED_FACE('',(#802,#445),#571,.T.);
#4322=ADVANCED_FACE('',(#803),#4121,.T.);
#4323=ADVANCED_FACE('',(#804,#446),#572,.T.);
#4324=ADVANCED_FACE('',(#805),#4122,.T.);
#4325=ADVANCED_FACE('',(#806,#447),#573,.T.);
#4326=ADVANCED_FACE('',(#807),#4123,.T.);
#4327=ADVANCED_FACE('',(#808,#448),#574,.T.);
#4328=ADVANCED_FACE('',(#809,#449),#4124,.F.);
#4329=ADVANCED_FACE('',(#810),#575,.F.);
#4330=ADVANCED_FACE('',(#811),#576,.F.);
#4331=ADVANCED_FACE('',(#812),#577,.F.);
#4332=ADVANCED_FACE('',(#813),#578,.F.);
#4333=ADVANCED_FACE('',(#814,#450),#579,.T.);
#4334=ADVANCED_FACE('',(#815,#451),#4125,.T.);
#4335=ADVANCED_FACE('',(#816,#452),#580,.T.);
#4336=ADVANCED_FACE('',(#817,#453),#4126,.F.);
#4337=ADVANCED_FACE('',(#818),#581,.T.);
#4338=ADVANCED_FACE('',(#819),#248,.T.);
#4339=ADVANCED_FACE('',(#820),#4127,.T.);
#4340=ADVANCED_FACE('',(#821),#249,.T.);
#4341=ADVANCED_FACE('',(#822,#454),#582,.T.);
#4342=ADVANCED_FACE('',(#823),#250,.T.);
#4343=ADVANCED_FACE('',(#824),#4128,.T.);
#4344=ADVANCED_FACE('',(#825),#251,.T.);
#4345=ADVANCED_FACE('',(#826),#583,.T.);
#4346=ADVANCED_FACE('',(#827),#584,.F.);
#4347=ADVANCED_FACE('',(#828),#585,.F.);
#4348=ADVANCED_FACE('',(#829),#586,.F.);
#4349=ADVANCED_FACE('',(#830),#587,.F.);
#4350=ADVANCED_FACE('',(#831),#588,.F.);
#4351=ADVANCED_FACE('',(#832),#589,.F.);
#4352=ADVANCED_FACE('',(#833),#590,.F.);
#4353=ADVANCED_FACE('',(#834),#591,.F.);
#4354=ADVANCED_FACE('',(#835),#592,.T.);
#4355=ADVANCED_FACE('',(#836),#252,.T.);
#4356=ADVANCED_FACE('',(#837),#4129,.T.);
#4357=ADVANCED_FACE('',(#838),#253,.T.);
#4358=ADVANCED_FACE('',(#839,#455),#593,.T.);
#4359=ADVANCED_FACE('',(#840),#254,.T.);
#4360=ADVANCED_FACE('',(#841),#4130,.T.);
#4361=ADVANCED_FACE('',(#842),#255,.T.);
#4362=ADVANCED_FACE('',(#843),#594,.T.);
#4363=ADVANCED_FACE('',(#844),#595,.F.);
#4364=ADVANCED_FACE('',(#845),#596,.F.);
#4365=ADVANCED_FACE('',(#846),#597,.F.);
#4366=ADVANCED_FACE('',(#847),#598,.F.);
#4367=ADVANCED_FACE('',(#848),#599,.F.);
#4368=ADVANCED_FACE('',(#849),#600,.F.);
#4369=ADVANCED_FACE('',(#850),#601,.F.);
#4370=ADVANCED_FACE('',(#851),#602,.F.);
#4371=ADVANCED_FACE('',(#852),#4131,.F.);
#4372=ADVANCED_FACE('',(#853),#4132,.T.);
#4373=ADVANCED_FACE('',(#854,#456),#603,.T.);
#4374=ADVANCED_FACE('',(#855,#457),#604,.F.);
#4375=ADVANCED_FACE('',(#856),#605,.T.);
#4376=ADVANCED_FACE('',(#857),#256,.T.);
#4377=ADVANCED_FACE('',(#858),#4133,.T.);
#4378=ADVANCED_FACE('',(#859),#257,.T.);
#4379=ADVANCED_FACE('',(#860,#458),#606,.T.);
#4380=ADVANCED_FACE('',(#861),#258,.T.);
#4381=ADVANCED_FACE('',(#862),#4134,.T.);
#4382=ADVANCED_FACE('',(#863),#259,.T.);
#4383=ADVANCED_FACE('',(#864),#607,.T.);
#4384=ADVANCED_FACE('',(#865),#608,.F.);
#4385=ADVANCED_FACE('',(#866),#609,.F.);
#4386=ADVANCED_FACE('',(#867),#610,.F.);
#4387=ADVANCED_FACE('',(#868),#611,.F.);
#4388=ADVANCED_FACE('',(#869),#612,.F.);
#4389=ADVANCED_FACE('',(#870),#613,.F.);
#4390=ADVANCED_FACE('',(#871),#614,.F.);
#4391=ADVANCED_FACE('',(#872),#615,.F.);
#4392=CLOSED_SHELL('',(#4135,#4136,#4137,#4138,#4139,#4140,#4141,#4142,
#4143,#4144,#4145,#4146,#4147,#4148,#4149,#4150,#4151,#4152));
#4393=CLOSED_SHELL('',(#4153,#4154,#4155,#4156,#4157,#4158,#4159,#4160,
#4161,#4162,#4163,#4164));
#4394=CLOSED_SHELL('',(#4165,#4166,#4167,#4168,#4169,#4170));
#4395=CLOSED_SHELL('',(#4171,#4172,#4173,#4174,#4175,#4176,#4177,#4178,
#4179,#4180,#4181,#4182));
#4396=CLOSED_SHELL('',(#4183,#4184,#4185,#4186,#4187,#4188));
#4397=CLOSED_SHELL('',(#4189,#4190,#4191,#4192,#4193));
#4398=CLOSED_SHELL('',(#4194,#4195,#4196,#4197,#4198,#4199,#4200,#4201,
#4202,#4203,#4204,#4205,#4206,#4207,#4208,#4209,#4210,#4211,#4212,#4213,
#4214,#4215,#4216));
#4399=CLOSED_SHELL('',(#4217,#4218,#4219,#4220,#4221,#4222,#4223,#4224));
#4400=CLOSED_SHELL('',(#4225,#4226,#4227,#4228,#4229,#4230,#4231,#4232));
#4401=CLOSED_SHELL('',(#4233,#4234,#4235,#4236,#4237,#4238,#4239,#4240,
#4241,#4242,#4243,#4244,#4245,#4246,#4247,#4248,#4249,#4250,#4251,#4252,
#4253,#4254,#4255,#4256,#4257,#4258,#4259,#4260,#4261,#4262,#4263,#4264));
#4402=CLOSED_SHELL('',(#4265,#4266,#4267,#4268));
#4403=CLOSED_SHELL('',(#4269,#4270,#4271,#4272));
#4404=CLOSED_SHELL('',(#4273,#4274,#4275,#4276,#4277,#4278,#4279,#4280,
#4281,#4282,#4283,#4284));
#4405=CLOSED_SHELL('',(#4285,#4286,#4287,#4288,#4289,#4290,#4291,#4292,
#4293,#4294,#4295,#4296));
#4406=CLOSED_SHELL('',(#4297,#4298,#4299,#4300,#4301,#4302,#4303,#4304,
#4305,#4306,#4307));
#4407=CLOSED_SHELL('',(#4308,#4309,#4310,#4311));
#4408=CLOSED_SHELL('',(#4312,#4313,#4314,#4315,#4316,#4317,#4318,#4319,
#4320,#4321,#4322,#4323,#4324,#4325,#4326,#4327,#4328));
#4409=CLOSED_SHELL('',(#4329,#4330,#4331,#4332,#4333,#4334,#4335,#4336));
#4410=CLOSED_SHELL('',(#4337,#4338,#4339,#4340,#4341,#4342,#4343,#4344,
#4345));
#4411=CLOSED_SHELL('',(#4346,#4347,#4348,#4349,#4350,#4351,#4352,#4353));
#4412=CLOSED_SHELL('',(#4354,#4355,#4356,#4357,#4358,#4359,#4360,#4361,
#4362));
#4413=CLOSED_SHELL('',(#4363,#4364,#4365,#4366,#4367,#4368,#4369,#4370));
#4414=CLOSED_SHELL('',(#4371,#4372,#4373,#4374));
#4415=CLOSED_SHELL('',(#4375,#4376,#4377,#4378,#4379,#4380,#4381,#4382,
#4383));
#4416=CLOSED_SHELL('',(#4384,#4385,#4386,#4387,#4388,#4389,#4390,#4391));
#4417=DERIVED_UNIT_ELEMENT(#4459,1.);
#4418=DERIVED_UNIT_ELEMENT(#7837,-3.);
#4419=DERIVED_UNIT_ELEMENT(#4459,1.);
#4420=DERIVED_UNIT_ELEMENT(#7837,-3.);
#4421=DERIVED_UNIT_ELEMENT(#4459,1.);
#4422=DERIVED_UNIT_ELEMENT(#7837,-3.);
#4423=DERIVED_UNIT_ELEMENT(#4459,1.);
#4424=DERIVED_UNIT_ELEMENT(#7837,-3.);
#4425=DERIVED_UNIT_ELEMENT(#4459,1.);
#4426=DERIVED_UNIT_ELEMENT(#7837,-3.);
#4427=DERIVED_UNIT_ELEMENT(#4459,1.);
#4428=DERIVED_UNIT_ELEMENT(#7837,-3.);
#4429=DERIVED_UNIT_ELEMENT(#4459,1.);
#4430=DERIVED_UNIT_ELEMENT(#7837,-3.);
#4431=DERIVED_UNIT_ELEMENT(#4459,1.);
#4432=DERIVED_UNIT_ELEMENT(#7837,-3.);
#4433=DERIVED_UNIT_ELEMENT(#4459,1.);
#4434=DERIVED_UNIT_ELEMENT(#7837,-3.);
#4435=DERIVED_UNIT_ELEMENT(#4459,1.);
#4436=DERIVED_UNIT_ELEMENT(#7837,-3.);
#4437=DERIVED_UNIT_ELEMENT(#4459,1.);
#4438=DERIVED_UNIT_ELEMENT(#7837,-3.);
#4439=DERIVED_UNIT_ELEMENT(#4459,1.);
#4440=DERIVED_UNIT_ELEMENT(#7837,-3.);
#4441=DERIVED_UNIT_ELEMENT(#4459,1.);
#4442=DERIVED_UNIT_ELEMENT(#7837,-3.);
#4443=DERIVED_UNIT_ELEMENT(#4459,1.);
#4444=DERIVED_UNIT_ELEMENT(#7837,-3.);
#4445=DERIVED_UNIT_ELEMENT(#4459,1.);
#4446=DERIVED_UNIT_ELEMENT(#7837,-3.);
#4447=DERIVED_UNIT_ELEMENT(#4459,1.);
#4448=DERIVED_UNIT_ELEMENT(#7837,-3.);
#4449=DERIVED_UNIT_ELEMENT(#4459,1.);
#4450=DERIVED_UNIT_ELEMENT(#7837,-3.);
#4451=DERIVED_UNIT_ELEMENT(#4459,1.);
#4452=DERIVED_UNIT_ELEMENT(#7837,-3.);
#4453=DERIVED_UNIT_ELEMENT(#4459,1.);
#4454=DERIVED_UNIT_ELEMENT(#7837,-3.);
#4455=DERIVED_UNIT_ELEMENT(#4459,1.);
#4456=DERIVED_UNIT_ELEMENT(#7837,-3.);
#4457=DERIVED_UNIT_ELEMENT(#4459,1.);
#4458=DERIVED_UNIT_ELEMENT(#7837,-3.);
#4459=(
MASS_UNIT()
NAMED_UNIT(*)
SI_UNIT(.KILO.,.GRAM.)
);
#4460=DERIVED_UNIT((#4417,#4418));
#4461=DERIVED_UNIT((#4419,#4420));
#4462=DERIVED_UNIT((#4421,#4422));
#4463=DERIVED_UNIT((#4423,#4424));
#4464=DERIVED_UNIT((#4425,#4426));
#4465=DERIVED_UNIT((#4427,#4428));
#4466=DERIVED_UNIT((#4429,#4430));
#4467=DERIVED_UNIT((#4431,#4432));
#4468=DERIVED_UNIT((#4433,#4434));
#4469=DERIVED_UNIT((#4435,#4436));
#4470=DERIVED_UNIT((#4437,#4438));
#4471=DERIVED_UNIT((#4439,#4440));
#4472=DERIVED_UNIT((#4441,#4442));
#4473=DERIVED_UNIT((#4443,#4444));
#4474=DERIVED_UNIT((#4445,#4446));
#4475=DERIVED_UNIT((#4447,#4448));
#4476=DERIVED_UNIT((#4449,#4450));
#4477=DERIVED_UNIT((#4451,#4452));
#4478=DERIVED_UNIT((#4453,#4454));
#4479=DERIVED_UNIT((#4455,#4456));
#4480=DERIVED_UNIT((#4457,#4458));
#4481=MEASURE_REPRESENTATION_ITEM('density measure',
POSITIVE_RATIO_MEASURE(7850.),#4460);
#4482=MEASURE_REPRESENTATION_ITEM('density measure',
POSITIVE_RATIO_MEASURE(7850.),#4461);
#4483=MEASURE_REPRESENTATION_ITEM('density measure',
POSITIVE_RATIO_MEASURE(7850.),#4462);
#4484=MEASURE_REPRESENTATION_ITEM('density measure',
POSITIVE_RATIO_MEASURE(7850.),#4463);
#4485=MEASURE_REPRESENTATION_ITEM('density measure',
POSITIVE_RATIO_MEASURE(7850.),#4464);
#4486=MEASURE_REPRESENTATION_ITEM('density measure',
POSITIVE_RATIO_MEASURE(7850.),#4465);
#4487=MEASURE_REPRESENTATION_ITEM('density measure',
POSITIVE_RATIO_MEASURE(7850.),#4466);
#4488=MEASURE_REPRESENTATION_ITEM('density measure',
POSITIVE_RATIO_MEASURE(7850.),#4467);
#4489=MEASURE_REPRESENTATION_ITEM('density measure',
POSITIVE_RATIO_MEASURE(7850.),#4468);
#4490=MEASURE_REPRESENTATION_ITEM('density measure',
POSITIVE_RATIO_MEASURE(7850.),#4469);
#4491=MEASURE_REPRESENTATION_ITEM('density measure',
POSITIVE_RATIO_MEASURE(7850.),#4470);
#4492=MEASURE_REPRESENTATION_ITEM('density measure',
POSITIVE_RATIO_MEASURE(7850.),#4471);
#4493=MEASURE_REPRESENTATION_ITEM('density measure',
POSITIVE_RATIO_MEASURE(7850.),#4472);
#4494=MEASURE_REPRESENTATION_ITEM('density measure',
POSITIVE_RATIO_MEASURE(7850.),#4473);
#4495=MEASURE_REPRESENTATION_ITEM('density measure',
POSITIVE_RATIO_MEASURE(7850.),#4474);
#4496=MEASURE_REPRESENTATION_ITEM('density measure',
POSITIVE_RATIO_MEASURE(7850.),#4475);
#4497=MEASURE_REPRESENTATION_ITEM('density measure',
POSITIVE_RATIO_MEASURE(7850.),#4476);
#4498=MEASURE_REPRESENTATION_ITEM('density measure',
POSITIVE_RATIO_MEASURE(7850.),#4477);
#4499=MEASURE_REPRESENTATION_ITEM('density measure',
POSITIVE_RATIO_MEASURE(7850.),#4478);
#4500=MEASURE_REPRESENTATION_ITEM('density measure',
POSITIVE_RATIO_MEASURE(7850.),#4479);
#4501=MEASURE_REPRESENTATION_ITEM('density measure',
POSITIVE_RATIO_MEASURE(7850.),#4480);
#4502=PROPERTY_DEFINITION_REPRESENTATION(#4607,#4544);
#4503=PROPERTY_DEFINITION_REPRESENTATION(#4608,#4545);
#4504=PROPERTY_DEFINITION_REPRESENTATION(#4609,#4546);
#4505=PROPERTY_DEFINITION_REPRESENTATION(#4610,#4547);
#4506=PROPERTY_DEFINITION_REPRESENTATION(#4611,#4548);
#4507=PROPERTY_DEFINITION_REPRESENTATION(#4612,#4549);
#4508=PROPERTY_DEFINITION_REPRESENTATION(#4613,#4550);
#4509=PROPERTY_DEFINITION_REPRESENTATION(#4614,#4551);
#4510=PROPERTY_DEFINITION_REPRESENTATION(#4615,#4552);
#4511=PROPERTY_DEFINITION_REPRESENTATION(#4616,#4553);
#4512=PROPERTY_DEFINITION_REPRESENTATION(#4617,#4554);
#4513=PROPERTY_DEFINITION_REPRESENTATION(#4618,#4555);
#4514=PROPERTY_DEFINITION_REPRESENTATION(#4619,#4556);
#4515=PROPERTY_DEFINITION_REPRESENTATION(#4620,#4557);
#4516=PROPERTY_DEFINITION_REPRESENTATION(#4621,#4558);
#4517=PROPERTY_DEFINITION_REPRESENTATION(#4622,#4559);
#4518=PROPERTY_DEFINITION_REPRESENTATION(#4623,#4560);
#4519=PROPERTY_DEFINITION_REPRESENTATION(#4624,#4561);
#4520=PROPERTY_DEFINITION_REPRESENTATION(#4625,#4562);
#4521=PROPERTY_DEFINITION_REPRESENTATION(#4626,#4563);
#4522=PROPERTY_DEFINITION_REPRESENTATION(#4627,#4564);
#4523=PROPERTY_DEFINITION_REPRESENTATION(#4628,#4565);
#4524=PROPERTY_DEFINITION_REPRESENTATION(#4629,#4566);
#4525=PROPERTY_DEFINITION_REPRESENTATION(#4630,#4567);
#4526=PROPERTY_DEFINITION_REPRESENTATION(#4631,#4568);
#4527=PROPERTY_DEFINITION_REPRESENTATION(#4632,#4569);
#4528=PROPERTY_DEFINITION_REPRESENTATION(#4633,#4570);
#4529=PROPERTY_DEFINITION_REPRESENTATION(#4634,#4571);
#4530=PROPERTY_DEFINITION_REPRESENTATION(#4635,#4572);
#4531=PROPERTY_DEFINITION_REPRESENTATION(#4636,#4573);
#4532=PROPERTY_DEFINITION_REPRESENTATION(#4637,#4574);
#4533=PROPERTY_DEFINITION_REPRESENTATION(#4638,#4575);
#4534=PROPERTY_DEFINITION_REPRESENTATION(#4639,#4576);
#4535=PROPERTY_DEFINITION_REPRESENTATION(#4640,#4577);
#4536=PROPERTY_DEFINITION_REPRESENTATION(#4641,#4578);
#4537=PROPERTY_DEFINITION_REPRESENTATION(#4642,#4579);
#4538=PROPERTY_DEFINITION_REPRESENTATION(#4643,#4580);
#4539=PROPERTY_DEFINITION_REPRESENTATION(#4644,#4581);
#4540=PROPERTY_DEFINITION_REPRESENTATION(#4645,#4582);
#4541=PROPERTY_DEFINITION_REPRESENTATION(#4646,#4583);
#4542=PROPERTY_DEFINITION_REPRESENTATION(#4647,#4584);
#4543=PROPERTY_DEFINITION_REPRESENTATION(#4648,#4585);
#4544=REPRESENTATION('material name',(#4586),#7812);
#4545=REPRESENTATION('density',(#4481),#7812);
#4546=REPRESENTATION('material name',(#4587),#7813);
#4547=REPRESENTATION('density',(#4482),#7813);
#4548=REPRESENTATION('material name',(#4588),#7814);
#4549=REPRESENTATION('density',(#4483),#7814);
#4550=REPRESENTATION('material name',(#4589),#7815);
#4551=REPRESENTATION('density',(#4484),#7815);
#4552=REPRESENTATION('material name',(#4590),#7816);
#4553=REPRESENTATION('density',(#4485),#7816);
#4554=REPRESENTATION('material name',(#4591),#7817);
#4555=REPRESENTATION('density',(#4486),#7817);
#4556=REPRESENTATION('material name',(#4592),#7818);
#4557=REPRESENTATION('density',(#4487),#7818);
#4558=REPRESENTATION('material name',(#4593),#7819);
#4559=REPRESENTATION('density',(#4488),#7819);
#4560=REPRESENTATION('material name',(#4594),#7821);
#4561=REPRESENTATION('density',(#4489),#7821);
#4562=REPRESENTATION('material name',(#4595),#7822);
#4563=REPRESENTATION('density',(#4490),#7822);
#4564=REPRESENTATION('material name',(#4596),#7823);
#4565=REPRESENTATION('density',(#4491),#7823);
#4566=REPRESENTATION('material name',(#4597),#7824);
#4567=REPRESENTATION('density',(#4492),#7824);
#4568=REPRESENTATION('material name',(#4598),#7825);
#4569=REPRESENTATION('density',(#4493),#7825);
#4570=REPRESENTATION('material name',(#4599),#7826);
#4571=REPRESENTATION('density',(#4494),#7826);
#4572=REPRESENTATION('material name',(#4600),#7827);
#4573=REPRESENTATION('density',(#4495),#7827);
#4574=REPRESENTATION('material name',(#4601),#7829);
#4575=REPRESENTATION('density',(#4496),#7829);
#4576=REPRESENTATION('material name',(#4602),#7830);
#4577=REPRESENTATION('density',(#4497),#7830);
#4578=REPRESENTATION('material name',(#4603),#7831);
#4579=REPRESENTATION('density',(#4498),#7831);
#4580=REPRESENTATION('material name',(#4604),#7832);
#4581=REPRESENTATION('density',(#4499),#7832);
#4582=REPRESENTATION('material name',(#4605),#7833);
#4583=REPRESENTATION('density',(#4500),#7833);
#4584=REPRESENTATION('material name',(#4606),#7834);
#4585=REPRESENTATION('density',(#4501),#7834);
#4586=DESCRIPTIVE_REPRESENTATION_ITEM('Steel','Steel');
#4587=DESCRIPTIVE_REPRESENTATION_ITEM('Steel','Steel');
#4588=DESCRIPTIVE_REPRESENTATION_ITEM('Steel','Steel');
#4589=DESCRIPTIVE_REPRESENTATION_ITEM('Steel','Steel');
#4590=DESCRIPTIVE_REPRESENTATION_ITEM('Steel','Steel');
#4591=DESCRIPTIVE_REPRESENTATION_ITEM('Steel','Steel');
#4592=DESCRIPTIVE_REPRESENTATION_ITEM('Steel','Steel');
#4593=DESCRIPTIVE_REPRESENTATION_ITEM('Steel','Steel');
#4594=DESCRIPTIVE_REPRESENTATION_ITEM('Steel','Steel');
#4595=DESCRIPTIVE_REPRESENTATION_ITEM('Steel','Steel');
#4596=DESCRIPTIVE_REPRESENTATION_ITEM('Steel','Steel');
#4597=DESCRIPTIVE_REPRESENTATION_ITEM('Steel','Steel');
#4598=DESCRIPTIVE_REPRESENTATION_ITEM('Steel','Steel');
#4599=DESCRIPTIVE_REPRESENTATION_ITEM('Steel','Steel');
#4600=DESCRIPTIVE_REPRESENTATION_ITEM('Steel','Steel');
#4601=DESCRIPTIVE_REPRESENTATION_ITEM('Steel','Steel');
#4602=DESCRIPTIVE_REPRESENTATION_ITEM('Steel','Steel');
#4603=DESCRIPTIVE_REPRESENTATION_ITEM('Steel','Steel');
#4604=DESCRIPTIVE_REPRESENTATION_ITEM('Steel','Steel');
#4605=DESCRIPTIVE_REPRESENTATION_ITEM('Steel','Steel');
#4606=DESCRIPTIVE_REPRESENTATION_ITEM('Steel','Steel');
#4607=PROPERTY_DEFINITION('material property','material name',#7974);
#4608=PROPERTY_DEFINITION('material property','density of part',#7974);
#4609=PROPERTY_DEFINITION('material property','material name',#7975);
#4610=PROPERTY_DEFINITION('material property','density of part',#7975);
#4611=PROPERTY_DEFINITION('material property','material name',#7976);
#4612=PROPERTY_DEFINITION('material property','density of part',#7976);
#4613=PROPERTY_DEFINITION('material property','material name',#7977);
#4614=PROPERTY_DEFINITION('material property','density of part',#7977);
#4615=PROPERTY_DEFINITION('material property','material name',#7978);
#4616=PROPERTY_DEFINITION('material property','density of part',#7978);
#4617=PROPERTY_DEFINITION('material property','material name',#7979);
#4618=PROPERTY_DEFINITION('material property','density of part',#7979);
#4619=PROPERTY_DEFINITION('material property','material name',#7980);
#4620=PROPERTY_DEFINITION('material property','density of part',#7980);
#4621=PROPERTY_DEFINITION('material property','material name',#7981);
#4622=PROPERTY_DEFINITION('material property','density of part',#7981);
#4623=PROPERTY_DEFINITION('material property','material name',#7983);
#4624=PROPERTY_DEFINITION('material property','density of part',#7983);
#4625=PROPERTY_DEFINITION('material property','material name',#7984);
#4626=PROPERTY_DEFINITION('material property','density of part',#7984);
#4627=PROPERTY_DEFINITION('material property','material name',#7985);
#4628=PROPERTY_DEFINITION('material property','density of part',#7985);
#4629=PROPERTY_DEFINITION('material property','material name',#7986);
#4630=PROPERTY_DEFINITION('material property','density of part',#7986);
#4631=PROPERTY_DEFINITION('material property','material name',#7987);
#4632=PROPERTY_DEFINITION('material property','density of part',#7987);
#4633=PROPERTY_DEFINITION('material property','material name',#7988);
#4634=PROPERTY_DEFINITION('material property','density of part',#7988);
#4635=PROPERTY_DEFINITION('material property','material name',#7989);
#4636=PROPERTY_DEFINITION('material property','density of part',#7989);
#4637=PROPERTY_DEFINITION('material property','material name',#7991);
#4638=PROPERTY_DEFINITION('material property','density of part',#7991);
#4639=PROPERTY_DEFINITION('material property','material name',#7992);
#4640=PROPERTY_DEFINITION('material property','density of part',#7992);
#4641=PROPERTY_DEFINITION('material property','material name',#7993);
#4642=PROPERTY_DEFINITION('material property','density of part',#7993);
#4643=PROPERTY_DEFINITION('material property','material name',#7994);
#4644=PROPERTY_DEFINITION('material property','density of part',#7994);
#4645=PROPERTY_DEFINITION('material property','material name',#7995);
#4646=PROPERTY_DEFINITION('material property','density of part',#7995);
#4647=PROPERTY_DEFINITION('material property','material name',#7996);
#4648=PROPERTY_DEFINITION('material property','density of part',#7996);
#4649=AXIS2_PLACEMENT_3D('',#6570,#5176,#5177);
#4650=AXIS2_PLACEMENT_3D('',#6571,#5178,#5179);
#4651=AXIS2_PLACEMENT_3D('',#6572,#5180,#5181);
#4652=AXIS2_PLACEMENT_3D('',#6573,#5182,#5183);
#4653=AXIS2_PLACEMENT_3D('',#6575,#5184,#5185);
#4654=AXIS2_PLACEMENT_3D('',#6578,#5187,#5188);
#4655=AXIS2_PLACEMENT_3D('',#6579,#5189,#5190);
#4656=AXIS2_PLACEMENT_3D('',#6581,#5191,#5192);
#4657=AXIS2_PLACEMENT_3D('',#6584,#5194,#5195);
#4658=AXIS2_PLACEMENT_3D('',#6585,#5196,#5197);
#4659=AXIS2_PLACEMENT_3D('',#6587,#5198,#5199);
#4660=AXIS2_PLACEMENT_3D('',#6590,#5201,#5202);
#4661=AXIS2_PLACEMENT_3D('',#6591,#5203,#5204);
#4662=AXIS2_PLACEMENT_3D('',#6593,#5205,#5206);
#4663=AXIS2_PLACEMENT_3D('',#6596,#5208,#5209);
#4664=AXIS2_PLACEMENT_3D('',#6597,#5210,#5211);
#4665=AXIS2_PLACEMENT_3D('',#6599,#5212,#5213);
#4666=AXIS2_PLACEMENT_3D('',#6602,#5215,#5216);
#4667=AXIS2_PLACEMENT_3D('',#6603,#5217,#5218);
#4668=AXIS2_PLACEMENT_3D('',#6605,#5219,#5220);
#4669=AXIS2_PLACEMENT_3D('',#6608,#5222,#5223);
#4670=AXIS2_PLACEMENT_3D('',#6609,#5224,#5225);
#4671=AXIS2_PLACEMENT_3D('',#6611,#5226,#5227);
#4672=AXIS2_PLACEMENT_3D('',#6614,#5229,#5230);
#4673=AXIS2_PLACEMENT_3D('',#6615,#5231,#5232);
#4674=AXIS2_PLACEMENT_3D('',#6617,#5233,#5234);
#4675=AXIS2_PLACEMENT_3D('',#6620,#5236,#5237);
#4676=AXIS2_PLACEMENT_3D('',#6621,#5238,#5239);
#4677=AXIS2_PLACEMENT_3D('',#6623,#5240,#5241);
#4678=AXIS2_PLACEMENT_3D('',#6626,#5243,#5244);
#4679=AXIS2_PLACEMENT_3D('',#6627,#5245,#5246);
#4680=AXIS2_PLACEMENT_3D('',#6629,#5247,#5248);
#4681=AXIS2_PLACEMENT_3D('',#6632,#5250,#5251);
#4682=AXIS2_PLACEMENT_3D('',#6633,#5252,#5253);
#4683=AXIS2_PLACEMENT_3D('',#6635,#5254,#5255);
#4684=AXIS2_PLACEMENT_3D('',#6638,#5257,#5258);
#4685=AXIS2_PLACEMENT_3D('',#6639,#5259,#5260);
#4686=AXIS2_PLACEMENT_3D('',#6641,#5261,#5262);
#4687=AXIS2_PLACEMENT_3D('',#6644,#5264,#5265);
#4688=AXIS2_PLACEMENT_3D('',#6645,#5266,#5267);
#4689=AXIS2_PLACEMENT_3D('',#6654,#5272,#5273);
#4690=AXIS2_PLACEMENT_3D('',#6660,#5277,#5278);
#4691=AXIS2_PLACEMENT_3D('',#6666,#5282,#5283);
#4692=AXIS2_PLACEMENT_3D('',#6669,#5286,#5287);
#4693=AXIS2_PLACEMENT_3D('',#6670,#5288,#5289);
#4694=AXIS2_PLACEMENT_3D('',#6671,#5290,#5291);
#4695=AXIS2_PLACEMENT_3D('',#6672,#5292,#5293);
#4696=AXIS2_PLACEMENT_3D('',#6674,#5294,#5295);
#4697=AXIS2_PLACEMENT_3D('',#6677,#5297,#5298);
#4698=AXIS2_PLACEMENT_3D('',#6678,#5299,#5300);
#4699=AXIS2_PLACEMENT_3D('',#6680,#5301,#5302);
#4700=AXIS2_PLACEMENT_3D('',#6681,#5303,#5304);
#4701=AXIS2_PLACEMENT_3D('',#6683,#5305,#5306);
#4702=AXIS2_PLACEMENT_3D('',#6686,#5308,#5309);
#4703=AXIS2_PLACEMENT_3D('',#6687,#5310,#5311);
#4704=AXIS2_PLACEMENT_3D('',#6689,#5312,#5313);
#4705=AXIS2_PLACEMENT_3D('',#6690,#5314,#5315);
#4706=AXIS2_PLACEMENT_3D('',#6692,#5316,#5317);
#4707=AXIS2_PLACEMENT_3D('',#6694,#5319,#5320);
#4708=AXIS2_PLACEMENT_3D('',#6696,#5321,#5322);
#4709=AXIS2_PLACEMENT_3D('',#6698,#5324,#5325);
#4710=AXIS2_PLACEMENT_3D('',#6707,#5330,#5331);
#4711=AXIS2_PLACEMENT_3D('',#6713,#5335,#5336);
#4712=AXIS2_PLACEMENT_3D('',#6719,#5340,#5341);
#4713=AXIS2_PLACEMENT_3D('',#6722,#5344,#5345);
#4714=AXIS2_PLACEMENT_3D('',#6723,#5346,#5347);
#4715=AXIS2_PLACEMENT_3D('',#6724,#5348,#5349);
#4716=AXIS2_PLACEMENT_3D('',#6725,#5350,#5351);
#4717=AXIS2_PLACEMENT_3D('',#6734,#5356,#5357);
#4718=AXIS2_PLACEMENT_3D('',#6740,#5361,#5362);
#4719=AXIS2_PLACEMENT_3D('',#6746,#5366,#5367);
#4720=AXIS2_PLACEMENT_3D('',#6749,#5370,#5371);
#4721=AXIS2_PLACEMENT_3D('',#6750,#5372,#5373);
#4722=AXIS2_PLACEMENT_3D('',#6751,#5374,#5375);
#4723=AXIS2_PLACEMENT_3D('',#6752,#5376,#5377);
#4724=AXIS2_PLACEMENT_3D('',#6754,#5378,#5379);
#4725=AXIS2_PLACEMENT_3D('',#6757,#5381,#5382);
#4726=AXIS2_PLACEMENT_3D('',#6758,#5383,#5384);
#4727=AXIS2_PLACEMENT_3D('',#6760,#5385,#5386);
#4728=AXIS2_PLACEMENT_3D('',#6761,#5387,#5388);
#4729=AXIS2_PLACEMENT_3D('',#6763,#5389,#5390);
#4730=AXIS2_PLACEMENT_3D('',#6766,#5392,#5393);
#4731=AXIS2_PLACEMENT_3D('',#6767,#5394,#5395);
#4732=AXIS2_PLACEMENT_3D('',#6769,#5396,#5397);
#4733=AXIS2_PLACEMENT_3D('',#6770,#5398,#5399);
#4734=AXIS2_PLACEMENT_3D('',#6772,#5400,#5401);
#4735=AXIS2_PLACEMENT_3D('',#6774,#5403,#5404);
#4736=AXIS2_PLACEMENT_3D('',#6776,#5405,#5406);
#4737=AXIS2_PLACEMENT_3D('',#6778,#5408,#5409);
#4738=AXIS2_PLACEMENT_3D('',#6787,#5414,#5415);
#4739=AXIS2_PLACEMENT_3D('',#6793,#5419,#5420);
#4740=AXIS2_PLACEMENT_3D('',#6799,#5424,#5425);
#4741=AXIS2_PLACEMENT_3D('',#6802,#5428,#5429);
#4742=AXIS2_PLACEMENT_3D('',#6803,#5430,#5431);
#4743=AXIS2_PLACEMENT_3D('',#6804,#5432,#5433);
#4744=AXIS2_PLACEMENT_3D('',#6805,#5434,#5435);
#4745=AXIS2_PLACEMENT_3D('',#6814,#5440,#5441);
#4746=AXIS2_PLACEMENT_3D('',#6820,#5445,#5446);
#4747=AXIS2_PLACEMENT_3D('',#6826,#5450,#5451);
#4748=AXIS2_PLACEMENT_3D('',#6829,#5454,#5455);
#4749=AXIS2_PLACEMENT_3D('',#6830,#5456,#5457);
#4750=AXIS2_PLACEMENT_3D('',#6831,#5458,#5459);
#4751=AXIS2_PLACEMENT_3D('',#6832,#5460,#5461);
#4752=AXIS2_PLACEMENT_3D('',#6834,#5462,#5463);
#4753=AXIS2_PLACEMENT_3D('',#6837,#5465,#5466);
#4754=AXIS2_PLACEMENT_3D('',#6838,#5467,#5468);
#4755=AXIS2_PLACEMENT_3D('',#6840,#5469,#5470);
#4756=AXIS2_PLACEMENT_3D('',#6842,#5472,#5473);
#4757=AXIS2_PLACEMENT_3D('',#6843,#5474,#5475);
#4758=AXIS2_PLACEMENT_3D('',#6845,#5476,#5477);
#4759=AXIS2_PLACEMENT_3D('',#6847,#5479,#5480);
#4760=AXIS2_PLACEMENT_3D('',#6848,#5481,#5482);
#4761=AXIS2_PLACEMENT_3D('',#6849,#5483,#5484);
#4762=AXIS2_PLACEMENT_3D('',#6853,#5486,#5487);
#4763=AXIS2_PLACEMENT_3D('',#6854,#5488,#5489);
#4764=AXIS2_PLACEMENT_3D('',#6858,#5491,#5492);
#4765=AXIS2_PLACEMENT_3D('',#6860,#5494,#5495);
#4766=AXIS2_PLACEMENT_3D('',#6865,#5497,#5498);
#4767=AXIS2_PLACEMENT_3D('',#6868,#5500,#5501);
#4768=AXIS2_PLACEMENT_3D('',#6869,#5502,#5503);
#4769=AXIS2_PLACEMENT_3D('',#6871,#5505,#5506);
#4770=AXIS2_PLACEMENT_3D('',#6882,#5512,#5513);
#4771=AXIS2_PLACEMENT_3D('',#6883,#5514,#5515);
#4772=AXIS2_PLACEMENT_3D('',#6890,#5519,#5520);
#4773=AXIS2_PLACEMENT_3D('',#6891,#5521,#5522);
#4774=AXIS2_PLACEMENT_3D('',#6902,#5528,#5529);
#4775=AXIS2_PLACEMENT_3D('',#6903,#5530,#5531);
#4776=AXIS2_PLACEMENT_3D('',#6905,#5532,#5533);
#4777=AXIS2_PLACEMENT_3D('',#6908,#5535,#5536);
#4778=AXIS2_PLACEMENT_3D('',#6909,#5537,#5538);
#4779=AXIS2_PLACEMENT_3D('',#6912,#5540,#5541);
#4780=AXIS2_PLACEMENT_3D('',#6913,#5542,#5543);
#4781=AXIS2_PLACEMENT_3D('',#6915,#5544,#5545);
#4782=AXIS2_PLACEMENT_3D('',#6917,#5547,#5548);
#4783=AXIS2_PLACEMENT_3D('',#6919,#5549,#5550);
#4784=AXIS2_PLACEMENT_3D('',#6921,#5552,#5553);
#4785=AXIS2_PLACEMENT_3D('',#6923,#5554,#5555);
#4786=AXIS2_PLACEMENT_3D('',#6926,#5557,#5558);
#4787=AXIS2_PLACEMENT_3D('',#6927,#5559,#5560);
#4788=AXIS2_PLACEMENT_3D('',#6944,#5570,#5571);
#4789=AXIS2_PLACEMENT_3D('',#6948,#5574,#5575);
#4790=AXIS2_PLACEMENT_3D('',#6952,#5578,#5579);
#4791=AXIS2_PLACEMENT_3D('',#6954,#5581,#5582);
#4792=AXIS2_PLACEMENT_3D('',#6958,#5585,#5586);
#4793=AXIS2_PLACEMENT_3D('',#6962,#5589,#5590);
#4794=AXIS2_PLACEMENT_3D('',#6966,#5593,#5594);
#4795=AXIS2_PLACEMENT_3D('',#6970,#5597,#5598);
#4796=AXIS2_PLACEMENT_3D('',#6974,#5601,#5602);
#4797=AXIS2_PLACEMENT_3D('',#6976,#5604,#5605);
#4798=AXIS2_PLACEMENT_3D('',#6977,#5606,#5607);
#4799=AXIS2_PLACEMENT_3D('',#6978,#5608,#5609);
#4800=AXIS2_PLACEMENT_3D('',#6987,#5614,#5615);
#4801=AXIS2_PLACEMENT_3D('',#6993,#5619,#5620);
#4802=AXIS2_PLACEMENT_3D('',#6999,#5624,#5625);
#4803=AXIS2_PLACEMENT_3D('',#7005,#5629,#5630);
#4804=AXIS2_PLACEMENT_3D('',#7011,#5634,#5635);
#4805=AXIS2_PLACEMENT_3D('',#7014,#5638,#5639);
#4806=AXIS2_PLACEMENT_3D('',#7015,#5640,#5641);
#4807=AXIS2_PLACEMENT_3D('',#7016,#5642,#5643);
#4808=AXIS2_PLACEMENT_3D('',#7018,#5644,#5645);
#4809=AXIS2_PLACEMENT_3D('',#7019,#5646,#5647);
#4810=AXIS2_PLACEMENT_3D('',#7021,#5648,#5649);
#4811=AXIS2_PLACEMENT_3D('',#7022,#5650,#5651);
#4812=AXIS2_PLACEMENT_3D('',#7024,#5652,#5653);
#4813=AXIS2_PLACEMENT_3D('',#7026,#5655,#5656);
#4814=AXIS2_PLACEMENT_3D('',#7028,#5657,#5658);
#4815=AXIS2_PLACEMENT_3D('',#7030,#5660,#5661);
#4816=AXIS2_PLACEMENT_3D('',#7032,#5662,#5663);
#4817=AXIS2_PLACEMENT_3D('',#7034,#5665,#5666);
#4818=AXIS2_PLACEMENT_3D('',#7036,#5667,#5668);
#4819=AXIS2_PLACEMENT_3D('',#7037,#5669,#5670);
#4820=AXIS2_PLACEMENT_3D('',#7039,#5671,#5672);
#4821=AXIS2_PLACEMENT_3D('',#7041,#5674,#5675);
#4822=AXIS2_PLACEMENT_3D('',#7043,#5677,#5678);
#4823=AXIS2_PLACEMENT_3D('',#7044,#5679,#5680);
#4824=AXIS2_PLACEMENT_3D('',#7045,#5681,#5682);
#4825=AXIS2_PLACEMENT_3D('',#7047,#5683,#5684);
#4826=AXIS2_PLACEMENT_3D('',#7050,#5686,#5687);
#4827=AXIS2_PLACEMENT_3D('',#7051,#5688,#5689);
#4828=AXIS2_PLACEMENT_3D('',#7052,#5690,#5691);
#4829=AXIS2_PLACEMENT_3D('',#7054,#5692,#5693);
#4830=AXIS2_PLACEMENT_3D('',#7057,#5695,#5696);
#4831=AXIS2_PLACEMENT_3D('',#7058,#5697,#5698);
#4832=AXIS2_PLACEMENT_3D('',#7059,#5699,#5700);
#4833=AXIS2_PLACEMENT_3D('',#7061,#5701,#5702);
#4834=AXIS2_PLACEMENT_3D('',#7064,#5704,#5705);
#4835=AXIS2_PLACEMENT_3D('',#7065,#5706,#5707);
#4836=AXIS2_PLACEMENT_3D('',#7066,#5708,#5709);
#4837=AXIS2_PLACEMENT_3D('',#7068,#5710,#5711);
#4838=AXIS2_PLACEMENT_3D('',#7071,#5713,#5714);
#4839=AXIS2_PLACEMENT_3D('',#7072,#5715,#5716);
#4840=AXIS2_PLACEMENT_3D('',#7073,#5717,#5718);
#4841=AXIS2_PLACEMENT_3D('',#7075,#5719,#5720);
#4842=AXIS2_PLACEMENT_3D('',#7078,#5722,#5723);
#4843=AXIS2_PLACEMENT_3D('',#7079,#5724,#5725);
#4844=AXIS2_PLACEMENT_3D('',#7080,#5726,#5727);
#4845=AXIS2_PLACEMENT_3D('',#7082,#5728,#5729);
#4846=AXIS2_PLACEMENT_3D('',#7085,#5731,#5732);
#4847=AXIS2_PLACEMENT_3D('',#7086,#5733,#5734);
#4848=AXIS2_PLACEMENT_3D('',#7087,#5735,#5736);
#4849=AXIS2_PLACEMENT_3D('',#7089,#5737,#5738);
#4850=AXIS2_PLACEMENT_3D('',#7092,#5740,#5741);
#4851=AXIS2_PLACEMENT_3D('',#7093,#5742,#5743);
#4852=AXIS2_PLACEMENT_3D('',#7094,#5744,#5745);
#4853=AXIS2_PLACEMENT_3D('',#7096,#5746,#5747);
#4854=AXIS2_PLACEMENT_3D('',#7099,#5749,#5750);
#4855=AXIS2_PLACEMENT_3D('',#7100,#5751,#5752);
#4856=AXIS2_PLACEMENT_3D('',#7101,#5753,#5754);
#4857=AXIS2_PLACEMENT_3D('',#7103,#5755,#5756);
#4858=AXIS2_PLACEMENT_3D('',#7106,#5758,#5759);
#4859=AXIS2_PLACEMENT_3D('',#7107,#5760,#5761);
#4860=AXIS2_PLACEMENT_3D('',#7108,#5762,#5763);
#4861=AXIS2_PLACEMENT_3D('',#7110,#5764,#5765);
#4862=AXIS2_PLACEMENT_3D('',#7113,#5767,#5768);
#4863=AXIS2_PLACEMENT_3D('',#7114,#5769,#5770);
#4864=AXIS2_PLACEMENT_3D('',#7115,#5771,#5772);
#4865=AXIS2_PLACEMENT_3D('',#7117,#5773,#5774);
#4866=AXIS2_PLACEMENT_3D('',#7120,#5776,#5777);
#4867=AXIS2_PLACEMENT_3D('',#7121,#5778,#5779);
#4868=AXIS2_PLACEMENT_3D('',#7122,#5780,#5781);
#4869=AXIS2_PLACEMENT_3D('',#7124,#5782,#5783);
#4870=AXIS2_PLACEMENT_3D('',#7127,#5785,#5786);
#4871=AXIS2_PLACEMENT_3D('',#7128,#5787,#5788);
#4872=AXIS2_PLACEMENT_3D('',#7129,#5789,#5790);
#4873=AXIS2_PLACEMENT_3D('',#7131,#5791,#5792);
#4874=AXIS2_PLACEMENT_3D('',#7134,#5794,#5795);
#4875=AXIS2_PLACEMENT_3D('',#7135,#5796,#5797);
#4876=AXIS2_PLACEMENT_3D('',#7137,#5798,#5799);
#4877=AXIS2_PLACEMENT_3D('',#7140,#5801,#5802);
#4878=AXIS2_PLACEMENT_3D('',#7141,#5803,#5804);
#4879=AXIS2_PLACEMENT_3D('',#7150,#5809,#5810);
#4880=AXIS2_PLACEMENT_3D('',#7156,#5814,#5815);
#4881=AXIS2_PLACEMENT_3D('',#7162,#5819,#5820);
#4882=AXIS2_PLACEMENT_3D('',#7165,#5823,#5824);
#4883=AXIS2_PLACEMENT_3D('',#7166,#5825,#5826);
#4884=AXIS2_PLACEMENT_3D('',#7167,#5827,#5828);
#4885=AXIS2_PLACEMENT_3D('',#7168,#5829,#5830);
#4886=AXIS2_PLACEMENT_3D('',#7170,#5831,#5832);
#4887=AXIS2_PLACEMENT_3D('',#7173,#5834,#5835);
#4888=AXIS2_PLACEMENT_3D('',#7174,#5836,#5837);
#4889=AXIS2_PLACEMENT_3D('',#7176,#5838,#5839);
#4890=AXIS2_PLACEMENT_3D('',#7179,#5841,#5842);
#4891=AXIS2_PLACEMENT_3D('',#7180,#5843,#5844);
#4892=AXIS2_PLACEMENT_3D('',#7181,#5845,#5846);
#4893=AXIS2_PLACEMENT_3D('',#7182,#5847,#5848);
#4894=AXIS2_PLACEMENT_3D('',#7183,#5849,#5850);
#4895=AXIS2_PLACEMENT_3D('',#7185,#5851,#5852);
#4896=AXIS2_PLACEMENT_3D('',#7188,#5854,#5855);
#4897=AXIS2_PLACEMENT_3D('',#7189,#5856,#5857);
#4898=AXIS2_PLACEMENT_3D('',#7191,#5858,#5859);
#4899=AXIS2_PLACEMENT_3D('',#7194,#5861,#5862);
#4900=AXIS2_PLACEMENT_3D('',#7195,#5863,#5864);
#4901=AXIS2_PLACEMENT_3D('',#7196,#5865,#5866);
#4902=AXIS2_PLACEMENT_3D('',#7197,#5867,#5868);
#4903=AXIS2_PLACEMENT_3D('',#7198,#5869,#5870);
#4904=AXIS2_PLACEMENT_3D('',#7200,#5871,#5872);
#4905=AXIS2_PLACEMENT_3D('',#7203,#5874,#5875);
#4906=AXIS2_PLACEMENT_3D('',#7204,#5876,#5877);
#4907=AXIS2_PLACEMENT_3D('',#7206,#5878,#5879);
#4908=AXIS2_PLACEMENT_3D('',#7209,#5881,#5882);
#4909=AXIS2_PLACEMENT_3D('',#7210,#5883,#5884);
#4910=AXIS2_PLACEMENT_3D('',#7212,#5885,#5886);
#4911=AXIS2_PLACEMENT_3D('',#7215,#5888,#5889);
#4912=AXIS2_PLACEMENT_3D('',#7216,#5890,#5891);
#4913=AXIS2_PLACEMENT_3D('',#7218,#5892,#5893);
#4914=AXIS2_PLACEMENT_3D('',#7221,#5895,#5896);
#4915=AXIS2_PLACEMENT_3D('',#7222,#5897,#5898);
#4916=AXIS2_PLACEMENT_3D('',#7224,#5899,#5900);
#4917=AXIS2_PLACEMENT_3D('',#7227,#5902,#5903);
#4918=AXIS2_PLACEMENT_3D('',#7228,#5904,#5905);
#4919=AXIS2_PLACEMENT_3D('',#7230,#5906,#5907);
#4920=AXIS2_PLACEMENT_3D('',#7233,#5909,#5910);
#4921=AXIS2_PLACEMENT_3D('',#7234,#5911,#5912);
#4922=AXIS2_PLACEMENT_3D('',#7243,#5917,#5918);
#4923=AXIS2_PLACEMENT_3D('',#7249,#5922,#5923);
#4924=AXIS2_PLACEMENT_3D('',#7255,#5927,#5928);
#4925=AXIS2_PLACEMENT_3D('',#7258,#5931,#5932);
#4926=AXIS2_PLACEMENT_3D('',#7259,#5933,#5934);
#4927=AXIS2_PLACEMENT_3D('',#7260,#5935,#5936);
#4928=AXIS2_PLACEMENT_3D('',#7261,#5937,#5938);
#4929=AXIS2_PLACEMENT_3D('',#7263,#5939,#5940);
#4930=AXIS2_PLACEMENT_3D('',#7266,#5942,#5943);
#4931=AXIS2_PLACEMENT_3D('',#7267,#5944,#5945);
#4932=AXIS2_PLACEMENT_3D('',#7269,#5946,#5947);
#4933=AXIS2_PLACEMENT_3D('',#7272,#5949,#5950);
#4934=AXIS2_PLACEMENT_3D('',#7273,#5951,#5952);
#4935=AXIS2_PLACEMENT_3D('',#7275,#5953,#5954);
#4936=AXIS2_PLACEMENT_3D('',#7278,#5956,#5957);
#4937=AXIS2_PLACEMENT_3D('',#7279,#5958,#5959);
#4938=AXIS2_PLACEMENT_3D('',#7281,#5960,#5961);
#4939=AXIS2_PLACEMENT_3D('',#7284,#5963,#5964);
#4940=AXIS2_PLACEMENT_3D('',#7285,#5965,#5966);
#4941=AXIS2_PLACEMENT_3D('',#7287,#5967,#5968);
#4942=AXIS2_PLACEMENT_3D('',#7290,#5970,#5971);
#4943=AXIS2_PLACEMENT_3D('',#7291,#5972,#5973);
#4944=AXIS2_PLACEMENT_3D('',#7293,#5974,#5975);
#4945=AXIS2_PLACEMENT_3D('',#7296,#5977,#5978);
#4946=AXIS2_PLACEMENT_3D('',#7297,#5979,#5980);
#4947=AXIS2_PLACEMENT_3D('',#7306,#5985,#5986);
#4948=AXIS2_PLACEMENT_3D('',#7312,#5990,#5991);
#4949=AXIS2_PLACEMENT_3D('',#7318,#5995,#5996);
#4950=AXIS2_PLACEMENT_3D('',#7321,#5999,#6000);
#4951=AXIS2_PLACEMENT_3D('',#7322,#6001,#6002);
#4952=AXIS2_PLACEMENT_3D('',#7323,#6003,#6004);
#4953=AXIS2_PLACEMENT_3D('',#7324,#6005,#6006);
#4954=AXIS2_PLACEMENT_3D('',#7326,#6007,#6008);
#4955=AXIS2_PLACEMENT_3D('',#7329,#6010,#6011);
#4956=AXIS2_PLACEMENT_3D('',#7330,#6012,#6013);
#4957=AXIS2_PLACEMENT_3D('',#7332,#6014,#6015);
#4958=AXIS2_PLACEMENT_3D('',#7335,#6017,#6018);
#4959=AXIS2_PLACEMENT_3D('',#7336,#6019,#6020);
#4960=AXIS2_PLACEMENT_3D('',#7338,#6021,#6022);
#4961=AXIS2_PLACEMENT_3D('',#7341,#6024,#6025);
#4962=AXIS2_PLACEMENT_3D('',#7342,#6026,#6027);
#4963=AXIS2_PLACEMENT_3D('',#7344,#6028,#6029);
#4964=AXIS2_PLACEMENT_3D('',#7347,#6031,#6032);
#4965=AXIS2_PLACEMENT_3D('',#7348,#6033,#6034);
#4966=AXIS2_PLACEMENT_3D('',#7350,#6035,#6036);
#4967=AXIS2_PLACEMENT_3D('',#7353,#6038,#6039);
#4968=AXIS2_PLACEMENT_3D('',#7354,#6040,#6041);
#4969=AXIS2_PLACEMENT_3D('',#7363,#6046,#6047);
#4970=AXIS2_PLACEMENT_3D('',#7369,#6051,#6052);
#4971=AXIS2_PLACEMENT_3D('',#7375,#6056,#6057);
#4972=AXIS2_PLACEMENT_3D('',#7378,#6060,#6061);
#4973=AXIS2_PLACEMENT_3D('',#7379,#6062,#6063);
#4974=AXIS2_PLACEMENT_3D('',#7380,#6064,#6065);
#4975=AXIS2_PLACEMENT_3D('',#7381,#6066,#6067);
#4976=AXIS2_PLACEMENT_3D('',#7383,#6068,#6069);
#4977=AXIS2_PLACEMENT_3D('',#7386,#6071,#6072);
#4978=AXIS2_PLACEMENT_3D('',#7387,#6073,#6074);
#4979=AXIS2_PLACEMENT_3D('',#7389,#6075,#6076);
#4980=AXIS2_PLACEMENT_3D('',#7392,#6078,#6079);
#4981=AXIS2_PLACEMENT_3D('',#7393,#6080,#6081);
#4982=AXIS2_PLACEMENT_3D('',#7394,#6082,#6083);
#4983=AXIS2_PLACEMENT_3D('',#7395,#6084,#6085);
#4984=AXIS2_PLACEMENT_3D('',#7396,#6086,#6087);
#4985=AXIS2_PLACEMENT_3D('',#7397,#6088,#6089);
#4986=AXIS2_PLACEMENT_3D('',#7400,#6090,#6091);
#4987=AXIS2_PLACEMENT_3D('',#7406,#6095,#6096);
#4988=AXIS2_PLACEMENT_3D('',#7412,#6100,#6101);
#4989=AXIS2_PLACEMENT_3D('',#7414,#6102,#6103);
#4990=AXIS2_PLACEMENT_3D('',#7418,#6106,#6107);
#4991=AXIS2_PLACEMENT_3D('',#7421,#6110,#6111);
#4992=AXIS2_PLACEMENT_3D('',#7422,#6112,#6113);
#4993=AXIS2_PLACEMENT_3D('',#7424,#6114,#6115);
#4994=AXIS2_PLACEMENT_3D('',#7426,#6116,#6117);
#4995=AXIS2_PLACEMENT_3D('',#7427,#6118,#6119);
#4996=AXIS2_PLACEMENT_3D('',#7429,#6120,#6121);
#4997=AXIS2_PLACEMENT_3D('',#7431,#6123,#6124);
#4998=AXIS2_PLACEMENT_3D('',#7433,#6125,#6126);
#4999=AXIS2_PLACEMENT_3D('',#7434,#6127,#6128);
#5000=AXIS2_PLACEMENT_3D('',#7436,#6129,#6130);
#5001=AXIS2_PLACEMENT_3D('',#7438,#6132,#6133);
#5002=AXIS2_PLACEMENT_3D('',#7440,#6134,#6135);
#5003=AXIS2_PLACEMENT_3D('',#7441,#6136,#6137);
#5004=AXIS2_PLACEMENT_3D('',#7443,#6138,#6139);
#5005=AXIS2_PLACEMENT_3D('',#7445,#6141,#6142);
#5006=AXIS2_PLACEMENT_3D('',#7447,#6143,#6144);
#5007=AXIS2_PLACEMENT_3D('',#7448,#6145,#6146);
#5008=AXIS2_PLACEMENT_3D('',#7450,#6147,#6148);
#5009=AXIS2_PLACEMENT_3D('',#7452,#6150,#6151);
#5010=AXIS2_PLACEMENT_3D('',#7454,#6152,#6153);
#5011=AXIS2_PLACEMENT_3D('',#7455,#6154,#6155);
#5012=AXIS2_PLACEMENT_3D('',#7457,#6156,#6157);
#5013=AXIS2_PLACEMENT_3D('',#7459,#6159,#6160);
#5014=AXIS2_PLACEMENT_3D('',#7461,#6161,#6162);
#5015=AXIS2_PLACEMENT_3D('',#7462,#6163,#6164);
#5016=AXIS2_PLACEMENT_3D('',#7464,#6166,#6167);
#5017=AXIS2_PLACEMENT_3D('',#7465,#6168,#6169);
#5018=AXIS2_PLACEMENT_3D('',#7468,#6170,#6171);
#5019=AXIS2_PLACEMENT_3D('',#7472,#6173,#6174);
#5020=AXIS2_PLACEMENT_3D('',#7474,#6176,#6177);
#5021=AXIS2_PLACEMENT_3D('',#7480,#6181,#6182);
#5022=AXIS2_PLACEMENT_3D('',#7482,#6183,#6184);
#5023=AXIS2_PLACEMENT_3D('',#7484,#6185,#6186);
#5024=AXIS2_PLACEMENT_3D('',#7486,#6188,#6189);
#5025=AXIS2_PLACEMENT_3D('',#7489,#6192,#6193);
#5026=AXIS2_PLACEMENT_3D('',#7491,#6194,#6195);
#5027=AXIS2_PLACEMENT_3D('',#7493,#6196,#6197);
#5028=AXIS2_PLACEMENT_3D('',#7494,#6198,#6199);
#5029=AXIS2_PLACEMENT_3D('',#7496,#6200,#6201);
#5030=AXIS2_PLACEMENT_3D('',#7498,#6203,#6204);
#5031=AXIS2_PLACEMENT_3D('',#7500,#6205,#6206);
#5032=AXIS2_PLACEMENT_3D('',#7501,#6207,#6208);
#5033=AXIS2_PLACEMENT_3D('',#7503,#6210,#6211);
#5034=AXIS2_PLACEMENT_3D('',#7504,#6212,#6213);
#5035=AXIS2_PLACEMENT_3D('',#7505,#6214,#6215);
#5036=AXIS2_PLACEMENT_3D('',#7506,#6216,#6217);
#5037=AXIS2_PLACEMENT_3D('',#7508,#6218,#6219);
#5038=AXIS2_PLACEMENT_3D('',#7509,#6220,#6221);
#5039=AXIS2_PLACEMENT_3D('',#7511,#6222,#6223);
#5040=AXIS2_PLACEMENT_3D('',#7513,#6225,#6226);
#5041=AXIS2_PLACEMENT_3D('',#7515,#6227,#6228);
#5042=AXIS2_PLACEMENT_3D('',#7517,#6230,#6231);
#5043=AXIS2_PLACEMENT_3D('',#7519,#6232,#6233);
#5044=AXIS2_PLACEMENT_3D('',#7521,#6235,#6236);
#5045=AXIS2_PLACEMENT_3D('',#7523,#6237,#6238);
#5046=AXIS2_PLACEMENT_3D('',#7524,#6239,#6240);
#5047=AXIS2_PLACEMENT_3D('',#7526,#6241,#6242);
#5048=AXIS2_PLACEMENT_3D('',#7528,#6244,#6245);
#5049=AXIS2_PLACEMENT_3D('',#7530,#6246,#6247);
#5050=AXIS2_PLACEMENT_3D('',#7532,#6249,#6250);
#5051=AXIS2_PLACEMENT_3D('',#7534,#6251,#6252);
#5052=AXIS2_PLACEMENT_3D('',#7536,#6254,#6255);
#5053=AXIS2_PLACEMENT_3D('',#7537,#6256,#6257);
#5054=AXIS2_PLACEMENT_3D('',#7546,#6262,#6263);
#5055=AXIS2_PLACEMENT_3D('',#7552,#6267,#6268);
#5056=AXIS2_PLACEMENT_3D('',#7558,#6272,#6273);
#5057=AXIS2_PLACEMENT_3D('',#7564,#6277,#6278);
#5058=AXIS2_PLACEMENT_3D('',#7570,#6282,#6283);
#5059=AXIS2_PLACEMENT_3D('',#7573,#6286,#6287);
#5060=AXIS2_PLACEMENT_3D('',#7574,#6288,#6289);
#5061=AXIS2_PLACEMENT_3D('',#7575,#6290,#6291);
#5062=AXIS2_PLACEMENT_3D('',#7576,#6292,#6293);
#5063=AXIS2_PLACEMENT_3D('',#7578,#6294,#6295);
#5064=AXIS2_PLACEMENT_3D('',#7579,#6296,#6297);
#5065=AXIS2_PLACEMENT_3D('',#7581,#6298,#6299);
#5066=AXIS2_PLACEMENT_3D('',#7583,#6301,#6302);
#5067=AXIS2_PLACEMENT_3D('',#7585,#6303,#6304);
#5068=AXIS2_PLACEMENT_3D('',#7587,#6306,#6307);
#5069=AXIS2_PLACEMENT_3D('',#7589,#6308,#6309);
#5070=AXIS2_PLACEMENT_3D('',#7591,#6311,#6312);
#5071=AXIS2_PLACEMENT_3D('',#7593,#6313,#6314);
#5072=AXIS2_PLACEMENT_3D('',#7594,#6315,#6316);
#5073=AXIS2_PLACEMENT_3D('',#7596,#6317,#6318);
#5074=AXIS2_PLACEMENT_3D('',#7598,#6320,#6321);
#5075=AXIS2_PLACEMENT_3D('',#7600,#6322,#6323);
#5076=AXIS2_PLACEMENT_3D('',#7602,#6325,#6326);
#5077=AXIS2_PLACEMENT_3D('',#7604,#6327,#6328);
#5078=AXIS2_PLACEMENT_3D('',#7606,#6330,#6331);
#5079=AXIS2_PLACEMENT_3D('',#7607,#6332,#6333);
#5080=AXIS2_PLACEMENT_3D('',#7616,#6338,#6339);
#5081=AXIS2_PLACEMENT_3D('',#7622,#6343,#6344);
#5082=AXIS2_PLACEMENT_3D('',#7628,#6348,#6349);
#5083=AXIS2_PLACEMENT_3D('',#7634,#6353,#6354);
#5084=AXIS2_PLACEMENT_3D('',#7640,#6358,#6359);
#5085=AXIS2_PLACEMENT_3D('',#7643,#6362,#6363);
#5086=AXIS2_PLACEMENT_3D('',#7644,#6364,#6365);
#5087=AXIS2_PLACEMENT_3D('',#7645,#6366,#6367);
#5088=AXIS2_PLACEMENT_3D('',#7646,#6368,#6369);
#5089=AXIS2_PLACEMENT_3D('',#7647,#6370,#6371);
#5090=AXIS2_PLACEMENT_3D('',#7648,#6372,#6373);
#5091=AXIS2_PLACEMENT_3D('',#7649,#6374,#6375);
#5092=AXIS2_PLACEMENT_3D('',#7650,#6376,#6377);
#5093=AXIS2_PLACEMENT_3D('',#7651,#6378,#6379);
#5094=AXIS2_PLACEMENT_3D('',#7652,#6380,#6381);
#5095=AXIS2_PLACEMENT_3D('',#7653,#6382,#6383);
#5096=AXIS2_PLACEMENT_3D('',#7654,#6384,#6385);
#5097=AXIS2_PLACEMENT_3D('',#7655,#6386,#6387);
#5098=AXIS2_PLACEMENT_3D('',#7656,#6388,#6389);
#5099=AXIS2_PLACEMENT_3D('',#7657,#6390,#6391);
#5100=AXIS2_PLACEMENT_3D('',#7658,#6392,#6393);
#5101=AXIS2_PLACEMENT_3D('',#7659,#6394,#6395);
#5102=AXIS2_PLACEMENT_3D('',#7660,#6396,#6397);
#5103=AXIS2_PLACEMENT_3D('',#7661,#6398,#6399);
#5104=AXIS2_PLACEMENT_3D('',#7662,#6400,#6401);
#5105=AXIS2_PLACEMENT_3D('',#7663,#6402,#6403);
#5106=AXIS2_PLACEMENT_3D('',#7664,#6404,#6405);
#5107=AXIS2_PLACEMENT_3D('',#7665,#6406,#6407);
#5108=AXIS2_PLACEMENT_3D('',#7666,#6408,#6409);
#5109=AXIS2_PLACEMENT_3D('',#7667,#6410,#6411);
#5110=AXIS2_PLACEMENT_3D('',#7668,#6412,#6413);
#5111=AXIS2_PLACEMENT_3D('',#7669,#6414,#6415);
#5112=AXIS2_PLACEMENT_3D('',#7670,#6416,#6417);
#5113=AXIS2_PLACEMENT_3D('',#7671,#6418,#6419);
#5114=AXIS2_PLACEMENT_3D('',#7672,#6420,#6421);
#5115=AXIS2_PLACEMENT_3D('',#7673,#6422,#6423);
#5116=AXIS2_PLACEMENT_3D('',#7675,#6424,#6425);
#5117=AXIS2_PLACEMENT_3D('',#7678,#6427,#6428);
#5118=AXIS2_PLACEMENT_3D('',#7679,#6429,#6430);
#5119=AXIS2_PLACEMENT_3D('',#7681,#6431,#6432);
#5120=AXIS2_PLACEMENT_3D('',#7684,#6434,#6435);
#5121=AXIS2_PLACEMENT_3D('',#7685,#6436,#6437);
#5122=AXIS2_PLACEMENT_3D('',#7686,#6438,#6439);
#5123=AXIS2_PLACEMENT_3D('',#7687,#6440,#6441);
#5124=AXIS2_PLACEMENT_3D('',#7688,#6442,#6443);
#5125=AXIS2_PLACEMENT_3D('',#7690,#6444,#6445);
#5126=AXIS2_PLACEMENT_3D('',#7691,#6446,#6447);
#5127=AXIS2_PLACEMENT_3D('',#7693,#6448,#6449);
#5128=AXIS2_PLACEMENT_3D('',#7695,#6451,#6452);
#5129=AXIS2_PLACEMENT_3D('',#7697,#6453,#6454);
#5130=AXIS2_PLACEMENT_3D('',#7699,#6456,#6457);
#5131=AXIS2_PLACEMENT_3D('',#7701,#6458,#6459);
#5132=AXIS2_PLACEMENT_3D('',#7703,#6461,#6462);
#5133=AXIS2_PLACEMENT_3D('',#7705,#6463,#6464);
#5134=AXIS2_PLACEMENT_3D('',#7706,#6465,#6466);
#5135=AXIS2_PLACEMENT_3D('',#7708,#6467,#6468);
#5136=AXIS2_PLACEMENT_3D('',#7710,#6470,#6471);
#5137=AXIS2_PLACEMENT_3D('',#7712,#6472,#6473);
#5138=AXIS2_PLACEMENT_3D('',#7714,#6475,#6476);
#5139=AXIS2_PLACEMENT_3D('',#7716,#6477,#6478);
#5140=AXIS2_PLACEMENT_3D('',#7718,#6480,#6481);
#5141=AXIS2_PLACEMENT_3D('',#7719,#6482,#6483);
#5142=AXIS2_PLACEMENT_3D('',#7728,#6488,#6489);
#5143=AXIS2_PLACEMENT_3D('',#7734,#6493,#6494);
#5144=AXIS2_PLACEMENT_3D('',#7740,#6498,#6499);
#5145=AXIS2_PLACEMENT_3D('',#7746,#6503,#6504);
#5146=AXIS2_PLACEMENT_3D('',#7752,#6508,#6509);
#5147=AXIS2_PLACEMENT_3D('',#7755,#6512,#6513);
#5148=AXIS2_PLACEMENT_3D('',#7756,#6514,#6515);
#5149=AXIS2_PLACEMENT_3D('',#7757,#6516,#6517);
#5150=AXIS2_PLACEMENT_3D('',#7758,#6518,#6519);
#5151=AXIS2_PLACEMENT_3D('',#7759,#6520,#6521);
#5152=AXIS2_PLACEMENT_3D('',#7760,#6522,#6523);
#5153=AXIS2_PLACEMENT_3D('',#7761,#6524,#6525);
#5154=AXIS2_PLACEMENT_3D('',#7762,#6526,#6527);
#5155=AXIS2_PLACEMENT_3D('',#7763,#6528,#6529);
#5156=AXIS2_PLACEMENT_3D('',#7764,#6530,#6531);
#5157=AXIS2_PLACEMENT_3D('',#7765,#6532,#6533);
#5158=AXIS2_PLACEMENT_3D('',#7766,#6534,#6535);
#5159=AXIS2_PLACEMENT_3D('',#7767,#6536,#6537);
#5160=AXIS2_PLACEMENT_3D('',#7768,#6538,#6539);
#5161=AXIS2_PLACEMENT_3D('',#7769,#6540,#6541);
#5162=AXIS2_PLACEMENT_3D('',#7770,#6542,#6543);
#5163=AXIS2_PLACEMENT_3D('',#7771,#6544,#6545);
#5164=AXIS2_PLACEMENT_3D('',#7772,#6546,#6547);
#5165=AXIS2_PLACEMENT_3D('',#7773,#6548,#6549);
#5166=AXIS2_PLACEMENT_3D('',#7774,#6550,#6551);
#5167=AXIS2_PLACEMENT_3D('',#7775,#6552,#6553);
#5168=AXIS2_PLACEMENT_3D('',#7776,#6554,#6555);
#5169=AXIS2_PLACEMENT_3D('',#7777,#6556,#6557);
#5170=AXIS2_PLACEMENT_3D('',#7778,#6558,#6559);
#5171=AXIS2_PLACEMENT_3D('',#7779,#6560,#6561);
#5172=AXIS2_PLACEMENT_3D('',#7780,#6562,#6563);
#5173=AXIS2_PLACEMENT_3D('',#7781,#6564,#6565);
#5174=AXIS2_PLACEMENT_3D('',#7782,#6566,#6567);
#5175=AXIS2_PLACEMENT_3D('',#7783,#6568,#6569);
#5176=DIRECTION('axis',(0.,0.,1.));
#5177=DIRECTION('refdir',(1.,0.,0.));
#5178=DIRECTION('axis',(0.,0.,1.));
#5179=DIRECTION('refdir',(1.,0.,0.));
#5180=DIRECTION('axis',(0.,0.,1.));
#5181=DIRECTION('refdir',(1.,0.,0.));
#5182=DIRECTION('center_axis',(0.,0.,1.));
#5183=DIRECTION('ref_axis',(1.,0.,0.));
#5184=DIRECTION('center_axis',(0.,0.,1.));
#5185=DIRECTION('ref_axis',(1.,0.,0.));
#5186=DIRECTION('',(0.,0.,1.));
#5187=DIRECTION('center_axis',(0.,0.,-1.));
#5188=DIRECTION('ref_axis',(1.,0.,0.));
#5189=DIRECTION('center_axis',(0.,0.,1.));
#5190=DIRECTION('ref_axis',(1.,0.,0.));
#5191=DIRECTION('center_axis',(0.,0.,1.));
#5192=DIRECTION('ref_axis',(1.,0.,0.));
#5193=DIRECTION('',(0.,0.,1.));
#5194=DIRECTION('center_axis',(0.,0.,-1.));
#5195=DIRECTION('ref_axis',(1.,0.,0.));
#5196=DIRECTION('center_axis',(0.,0.,1.));
#5197=DIRECTION('ref_axis',(1.,0.,0.));
#5198=DIRECTION('center_axis',(0.,0.,1.));
#5199=DIRECTION('ref_axis',(1.,0.,0.));
#5200=DIRECTION('',(0.,0.,1.));
#5201=DIRECTION('center_axis',(0.,0.,-1.));
#5202=DIRECTION('ref_axis',(1.,0.,0.));
#5203=DIRECTION('center_axis',(0.,0.,1.));
#5204=DIRECTION('ref_axis',(1.,0.,0.));
#5205=DIRECTION('center_axis',(0.,0.,1.));
#5206=DIRECTION('ref_axis',(1.,0.,0.));
#5207=DIRECTION('',(0.,0.,1.));
#5208=DIRECTION('center_axis',(0.,0.,-1.));
#5209=DIRECTION('ref_axis',(1.,0.,0.));
#5210=DIRECTION('center_axis',(0.,0.,1.));
#5211=DIRECTION('ref_axis',(1.,0.,0.));
#5212=DIRECTION('center_axis',(0.,0.,1.));
#5213=DIRECTION('ref_axis',(1.,0.,0.));
#5214=DIRECTION('',(0.,0.,1.));
#5215=DIRECTION('center_axis',(0.,0.,-1.));
#5216=DIRECTION('ref_axis',(1.,0.,0.));
#5217=DIRECTION('center_axis',(0.,0.,1.));
#5218=DIRECTION('ref_axis',(1.,0.,0.));
#5219=DIRECTION('center_axis',(0.,0.,1.));
#5220=DIRECTION('ref_axis',(1.,0.,0.));
#5221=DIRECTION('',(0.,0.,1.));
#5222=DIRECTION('center_axis',(0.,0.,-1.));
#5223=DIRECTION('ref_axis',(1.,0.,0.));
#5224=DIRECTION('center_axis',(0.,0.,1.));
#5225=DIRECTION('ref_axis',(1.,0.,0.));
#5226=DIRECTION('center_axis',(0.,0.,1.));
#5227=DIRECTION('ref_axis',(1.,0.,0.));
#5228=DIRECTION('',(0.,0.,1.));
#5229=DIRECTION('center_axis',(0.,0.,-1.));
#5230=DIRECTION('ref_axis',(1.,0.,0.));
#5231=DIRECTION('center_axis',(0.,0.,1.));
#5232=DIRECTION('ref_axis',(1.,0.,0.));
#5233=DIRECTION('center_axis',(0.,0.,1.));
#5234=DIRECTION('ref_axis',(1.,0.,0.));
#5235=DIRECTION('',(0.,0.,1.));
#5236=DIRECTION('center_axis',(0.,0.,-1.));
#5237=DIRECTION('ref_axis',(1.,0.,0.));
#5238=DIRECTION('center_axis',(0.,0.,1.));
#5239=DIRECTION('ref_axis',(1.,0.,0.));
#5240=DIRECTION('center_axis',(0.,0.,1.));
#5241=DIRECTION('ref_axis',(1.,0.,0.));
#5242=DIRECTION('',(0.,0.,1.));
#5243=DIRECTION('center_axis',(0.,0.,-1.));
#5244=DIRECTION('ref_axis',(1.,0.,0.));
#5245=DIRECTION('center_axis',(0.,0.,1.));
#5246=DIRECTION('ref_axis',(1.,0.,0.));
#5247=DIRECTION('center_axis',(0.,0.,1.));
#5248=DIRECTION('ref_axis',(1.,0.,0.));
#5249=DIRECTION('',(0.,0.,1.));
#5250=DIRECTION('center_axis',(0.,0.,-1.));
#5251=DIRECTION('ref_axis',(1.,0.,0.));
#5252=DIRECTION('center_axis',(0.,0.,1.));
#5253=DIRECTION('ref_axis',(1.,0.,0.));
#5254=DIRECTION('center_axis',(0.,0.,1.));
#5255=DIRECTION('ref_axis',(1.,0.,0.));
#5256=DIRECTION('',(0.,0.,1.));
#5257=DIRECTION('center_axis',(0.,0.,-1.));
#5258=DIRECTION('ref_axis',(1.,0.,0.));
#5259=DIRECTION('center_axis',(0.,0.,1.));
#5260=DIRECTION('ref_axis',(1.,0.,0.));
#5261=DIRECTION('center_axis',(0.,0.,1.));
#5262=DIRECTION('ref_axis',(1.,0.,0.));
#5263=DIRECTION('',(0.,0.,1.));
#5264=DIRECTION('center_axis',(0.,0.,-1.));
#5265=DIRECTION('ref_axis',(1.,0.,0.));
#5266=DIRECTION('center_axis',(0.,1.,0.));
#5267=DIRECTION('ref_axis',(-1.,0.,0.));
#5268=DIRECTION('',(-1.,0.,0.));
#5269=DIRECTION('',(0.,0.,1.));
#5270=DIRECTION('',(-1.,0.,0.));
#5271=DIRECTION('',(0.,0.,1.));
#5272=DIRECTION('center_axis',(1.,0.,0.));
#5273=DIRECTION('ref_axis',(0.,1.,0.));
#5274=DIRECTION('',(0.,1.,0.));
#5275=DIRECTION('',(0.,1.,0.));
#5276=DIRECTION('',(0.,0.,1.));
#5277=DIRECTION('center_axis',(0.,-1.,0.));
#5278=DIRECTION('ref_axis',(1.,0.,0.));
#5279=DIRECTION('',(1.,0.,0.));
#5280=DIRECTION('',(1.,0.,0.));
#5281=DIRECTION('',(0.,0.,1.));
#5282=DIRECTION('center_axis',(-1.,0.,0.));
#5283=DIRECTION('ref_axis',(0.,-1.,0.));
#5284=DIRECTION('',(0.,-1.,0.));
#5285=DIRECTION('',(0.,-1.,0.));
#5286=DIRECTION('center_axis',(0.,0.,1.));
#5287=DIRECTION('ref_axis',(1.,0.,0.));
#5288=DIRECTION('center_axis',(0.,0.,1.));
#5289=DIRECTION('ref_axis',(1.,0.,0.));
#5290=DIRECTION('axis',(0.,0.,1.));
#5291=DIRECTION('refdir',(1.,0.,0.));
#5292=DIRECTION('center_axis',(0.,0.,1.));
#5293=DIRECTION('ref_axis',(1.,0.,0.));
#5294=DIRECTION('center_axis',(0.,0.,1.));
#5295=DIRECTION('ref_axis',(1.,0.,0.));
#5296=DIRECTION('',(0.,0.,1.));
#5297=DIRECTION('center_axis',(0.,0.,-1.));
#5298=DIRECTION('ref_axis',(1.,0.,0.));
#5299=DIRECTION('center_axis',(0.,0.,1.));
#5300=DIRECTION('ref_axis',(1.,0.,0.));
#5301=DIRECTION('center_axis',(0.,0.,1.));
#5302=DIRECTION('ref_axis',(1.,0.,0.));
#5303=DIRECTION('center_axis',(0.,0.,1.));
#5304=DIRECTION('ref_axis',(1.,0.,0.));
#5305=DIRECTION('center_axis',(0.,0.,1.));
#5306=DIRECTION('ref_axis',(1.,0.,0.));
#5307=DIRECTION('',(0.,0.,1.));
#5308=DIRECTION('center_axis',(0.,0.,-1.));
#5309=DIRECTION('ref_axis',(1.,0.,0.));
#5310=DIRECTION('center_axis',(0.,0.,1.));
#5311=DIRECTION('ref_axis',(1.,0.,0.));
#5312=DIRECTION('center_axis',(0.,0.,1.));
#5313=DIRECTION('ref_axis',(1.,0.,0.));
#5314=DIRECTION('center_axis',(0.,0.,1.));
#5315=DIRECTION('ref_axis',(1.,0.,0.));
#5316=DIRECTION('center_axis',(0.,0.,1.));
#5317=DIRECTION('ref_axis',(1.,0.,0.));
#5318=DIRECTION('',(0.,0.,1.));
#5319=DIRECTION('center_axis',(0.,0.,1.));
#5320=DIRECTION('ref_axis',(1.,0.,0.));
#5321=DIRECTION('center_axis',(0.,0.,1.));
#5322=DIRECTION('ref_axis',(1.,0.,0.));
#5323=DIRECTION('',(0.,0.,1.));
#5324=DIRECTION('center_axis',(0.,1.,0.));
#5325=DIRECTION('ref_axis',(-1.,0.,0.));
#5326=DIRECTION('',(-1.,0.,0.));
#5327=DIRECTION('',(0.,0.,1.));
#5328=DIRECTION('',(-1.,0.,0.));
#5329=DIRECTION('',(0.,0.,1.));
#5330=DIRECTION('center_axis',(1.,0.,0.));
#5331=DIRECTION('ref_axis',(0.,1.,0.));
#5332=DIRECTION('',(0.,1.,0.));
#5333=DIRECTION('',(0.,1.,0.));
#5334=DIRECTION('',(0.,0.,1.));
#5335=DIRECTION('center_axis',(0.,-1.,0.));
#5336=DIRECTION('ref_axis',(1.,0.,0.));
#5337=DIRECTION('',(1.,0.,0.));
#5338=DIRECTION('',(1.,0.,0.));
#5339=DIRECTION('',(0.,0.,1.));
#5340=DIRECTION('center_axis',(-1.,0.,0.));
#5341=DIRECTION('ref_axis',(0.,-1.,0.));
#5342=DIRECTION('',(0.,-1.,0.));
#5343=DIRECTION('',(0.,-1.,0.));
#5344=DIRECTION('center_axis',(0.,0.,1.));
#5345=DIRECTION('ref_axis',(1.,0.,0.));
#5346=DIRECTION('center_axis',(0.,0.,1.));
#5347=DIRECTION('ref_axis',(1.,0.,0.));
#5348=DIRECTION('axis',(0.,0.,1.));
#5349=DIRECTION('refdir',(1.,0.,0.));
#5350=DIRECTION('center_axis',(0.,1.,0.));
#5351=DIRECTION('ref_axis',(-1.,0.,0.));
#5352=DIRECTION('',(-1.,0.,0.));
#5353=DIRECTION('',(0.,0.,1.));
#5354=DIRECTION('',(-1.,0.,0.));
#5355=DIRECTION('',(0.,0.,1.));
#5356=DIRECTION('center_axis',(1.,0.,0.));
#5357=DIRECTION('ref_axis',(0.,1.,0.));
#5358=DIRECTION('',(0.,1.,0.));
#5359=DIRECTION('',(0.,1.,0.));
#5360=DIRECTION('',(0.,0.,1.));
#5361=DIRECTION('center_axis',(0.,-1.,0.));
#5362=DIRECTION('ref_axis',(1.,0.,0.));
#5363=DIRECTION('',(1.,0.,0.));
#5364=DIRECTION('',(1.,0.,0.));
#5365=DIRECTION('',(0.,0.,1.));
#5366=DIRECTION('center_axis',(-1.,0.,0.));
#5367=DIRECTION('ref_axis',(0.,-1.,0.));
#5368=DIRECTION('',(0.,-1.,0.));
#5369=DIRECTION('',(0.,-1.,0.));
#5370=DIRECTION('center_axis',(0.,0.,1.));
#5371=DIRECTION('ref_axis',(1.,0.,0.));
#5372=DIRECTION('center_axis',(0.,0.,1.));
#5373=DIRECTION('ref_axis',(1.,0.,0.));
#5374=DIRECTION('axis',(0.,0.,1.));
#5375=DIRECTION('refdir',(1.,0.,0.));
#5376=DIRECTION('center_axis',(0.,0.,1.));
#5377=DIRECTION('ref_axis',(1.,0.,0.));
#5378=DIRECTION('center_axis',(0.,0.,1.));
#5379=DIRECTION('ref_axis',(1.,0.,0.));
#5380=DIRECTION('',(0.,0.,1.));
#5381=DIRECTION('center_axis',(0.,0.,-1.));
#5382=DIRECTION('ref_axis',(1.,0.,0.));
#5383=DIRECTION('center_axis',(0.,0.,1.));
#5384=DIRECTION('ref_axis',(1.,0.,0.));
#5385=DIRECTION('center_axis',(0.,0.,1.));
#5386=DIRECTION('ref_axis',(1.,0.,0.));
#5387=DIRECTION('center_axis',(0.,0.,1.));
#5388=DIRECTION('ref_axis',(1.,0.,0.));
#5389=DIRECTION('center_axis',(0.,0.,1.));
#5390=DIRECTION('ref_axis',(1.,0.,0.));
#5391=DIRECTION('',(0.,0.,1.));
#5392=DIRECTION('center_axis',(0.,0.,-1.));
#5393=DIRECTION('ref_axis',(1.,0.,0.));
#5394=DIRECTION('center_axis',(0.,0.,1.));
#5395=DIRECTION('ref_axis',(1.,0.,0.));
#5396=DIRECTION('center_axis',(0.,0.,1.));
#5397=DIRECTION('ref_axis',(1.,0.,0.));
#5398=DIRECTION('center_axis',(0.,0.,1.));
#5399=DIRECTION('ref_axis',(1.,0.,0.));
#5400=DIRECTION('center_axis',(0.,0.,1.));
#5401=DIRECTION('ref_axis',(1.,0.,0.));
#5402=DIRECTION('',(0.,0.,1.));
#5403=DIRECTION('center_axis',(0.,0.,1.));
#5404=DIRECTION('ref_axis',(1.,0.,0.));
#5405=DIRECTION('center_axis',(0.,0.,1.));
#5406=DIRECTION('ref_axis',(1.,0.,0.));
#5407=DIRECTION('',(0.,0.,1.));
#5408=DIRECTION('center_axis',(0.,1.,0.));
#5409=DIRECTION('ref_axis',(-1.,0.,0.));
#5410=DIRECTION('',(-1.,0.,0.));
#5411=DIRECTION('',(0.,0.,1.));
#5412=DIRECTION('',(-1.,0.,0.));
#5413=DIRECTION('',(0.,0.,1.));
#5414=DIRECTION('center_axis',(1.,0.,0.));
#5415=DIRECTION('ref_axis',(0.,1.,0.));
#5416=DIRECTION('',(0.,1.,0.));
#5417=DIRECTION('',(0.,1.,0.));
#5418=DIRECTION('',(0.,0.,1.));
#5419=DIRECTION('center_axis',(0.,-1.,0.));
#5420=DIRECTION('ref_axis',(1.,0.,0.));
#5421=DIRECTION('',(1.,0.,0.));
#5422=DIRECTION('',(1.,0.,0.));
#5423=DIRECTION('',(0.,0.,1.));
#5424=DIRECTION('center_axis',(-1.,0.,0.));
#5425=DIRECTION('ref_axis',(0.,-1.,0.));
#5426=DIRECTION('',(0.,-1.,0.));
#5427=DIRECTION('',(0.,-1.,0.));
#5428=DIRECTION('center_axis',(0.,0.,1.));
#5429=DIRECTION('ref_axis',(1.,0.,0.));
#5430=DIRECTION('center_axis',(0.,0.,1.));
#5431=DIRECTION('ref_axis',(1.,0.,0.));
#5432=DIRECTION('axis',(0.,0.,1.));
#5433=DIRECTION('refdir',(1.,0.,0.));
#5434=DIRECTION('center_axis',(0.,1.,0.));
#5435=DIRECTION('ref_axis',(-1.,0.,0.));
#5436=DIRECTION('',(-1.,0.,0.));
#5437=DIRECTION('',(0.,0.,1.));
#5438=DIRECTION('',(-1.,0.,0.));
#5439=DIRECTION('',(0.,0.,1.));
#5440=DIRECTION('center_axis',(1.,0.,0.));
#5441=DIRECTION('ref_axis',(0.,1.,0.));
#5442=DIRECTION('',(0.,1.,0.));
#5443=DIRECTION('',(0.,1.,0.));
#5444=DIRECTION('',(0.,0.,1.));
#5445=DIRECTION('center_axis',(0.,-1.,0.));
#5446=DIRECTION('ref_axis',(1.,0.,0.));
#5447=DIRECTION('',(1.,0.,0.));
#5448=DIRECTION('',(1.,0.,0.));
#5449=DIRECTION('',(0.,0.,1.));
#5450=DIRECTION('center_axis',(-1.,0.,0.));
#5451=DIRECTION('ref_axis',(0.,-1.,0.));
#5452=DIRECTION('',(0.,-1.,0.));
#5453=DIRECTION('',(0.,-1.,0.));
#5454=DIRECTION('center_axis',(0.,0.,1.));
#5455=DIRECTION('ref_axis',(1.,0.,0.));
#5456=DIRECTION('center_axis',(0.,0.,1.));
#5457=DIRECTION('ref_axis',(1.,0.,0.));
#5458=DIRECTION('axis',(0.,0.,1.));
#5459=DIRECTION('refdir',(1.,0.,0.));
#5460=DIRECTION('center_axis',(1.,0.,0.));
#5461=DIRECTION('ref_axis',(0.,0.,-1.));
#5462=DIRECTION('center_axis',(-1.,0.,0.));
#5463=DIRECTION('ref_axis',(0.,0.,-1.));
#5464=DIRECTION('',(-0.707106781186548,8.65956056235493E-17,-0.707106781186547));
#5465=DIRECTION('center_axis',(1.,0.,0.));
#5466=DIRECTION('ref_axis',(0.,0.,-1.));
#5467=DIRECTION('center_axis',(1.,0.,0.));
#5468=DIRECTION('ref_axis',(0.,0.,-1.));
#5469=DIRECTION('center_axis',(1.,0.,0.));
#5470=DIRECTION('ref_axis',(0.,0.,-1.));
#5471=DIRECTION('',(-1.,0.,0.));
#5472=DIRECTION('center_axis',(1.,0.,0.));
#5473=DIRECTION('ref_axis',(0.,0.,-1.));
#5474=DIRECTION('center_axis',(-1.,0.,0.));
#5475=DIRECTION('ref_axis',(0.,0.,-1.));
#5476=DIRECTION('center_axis',(-1.,0.,0.));
#5477=DIRECTION('ref_axis',(0.,0.,-1.));
#5478=DIRECTION('',(-0.707106781186553,-8.65956056235487E-17,0.707106781186542));
#5479=DIRECTION('center_axis',(1.,0.,0.));
#5480=DIRECTION('ref_axis',(0.,0.,-1.));
#5481=DIRECTION('axis',(0.,0.,1.));
#5482=DIRECTION('refdir',(1.,0.,0.));
#5483=DIRECTION('center_axis',(0.,0.,1.));
#5484=DIRECTION('ref_axis',(1.,0.,0.));
#5485=DIRECTION('',(0.,-1.,0.));
#5486=DIRECTION('center_axis',(0.,0.,1.));
#5487=DIRECTION('ref_axis',(1.,0.,0.));
#5488=DIRECTION('center_axis',(0.,0.,1.));
#5489=DIRECTION('ref_axis',(1.,0.,0.));
#5490=DIRECTION('',(0.,0.,1.));
#5491=DIRECTION('center_axis',(0.,0.,1.));
#5492=DIRECTION('ref_axis',(1.,0.,0.));
#5493=DIRECTION('',(0.,0.,-1.));
#5494=DIRECTION('center_axis',(0.,0.,1.));
#5495=DIRECTION('ref_axis',(-1.,1.22464679914735E-16,0.));
#5496=DIRECTION('',(0.,0.,-1.));
#5497=DIRECTION('center_axis',(0.,0.,1.));
#5498=DIRECTION('ref_axis',(1.,0.,0.));
#5499=DIRECTION('',(0.,0.,1.));
#5500=DIRECTION('center_axis',(0.,0.,1.));
#5501=DIRECTION('ref_axis',(1.,0.,0.));
#5502=DIRECTION('center_axis',(0.,0.,1.));
#5503=DIRECTION('ref_axis',(1.,0.,0.));
#5504=DIRECTION('',(0.,1.,0.));
#5505=DIRECTION('center_axis',(0.,0.,1.));
#5506=DIRECTION('ref_axis',(1.,0.,0.));
#5507=DIRECTION('',(0.,1.,0.));
#5508=DIRECTION('',(1.,0.,0.));
#5509=DIRECTION('',(0.,-1.,0.));
#5510=DIRECTION('',(-1.,0.,0.));
#5511=DIRECTION('',(0.,1.,0.));
#5512=DIRECTION('center_axis',(0.,0.,-1.));
#5513=DIRECTION('ref_axis',(1.,0.,0.));
#5514=DIRECTION('center_axis',(-1.,0.,0.));
#5515=DIRECTION('ref_axis',(0.,0.,1.));
#5516=DIRECTION('',(0.,0.,-1.));
#5517=DIRECTION('',(0.,1.,0.));
#5518=DIRECTION('',(0.,0.,1.));
#5519=DIRECTION('center_axis',(1.,0.,0.));
#5520=DIRECTION('ref_axis',(0.,0.,-1.));
#5521=DIRECTION('center_axis',(0.,0.,1.));
#5522=DIRECTION('ref_axis',(1.,0.,0.));
#5523=DIRECTION('',(0.,1.,0.));
#5524=DIRECTION('',(1.,0.,0.));
#5525=DIRECTION('',(0.,1.,0.));
#5526=DIRECTION('',(0.,1.,0.));
#5527=DIRECTION('',(-1.,0.,0.));
#5528=DIRECTION('center_axis',(0.,0.,-1.));
#5529=DIRECTION('ref_axis',(1.,0.,0.));
#5530=DIRECTION('center_axis',(1.,0.,0.));
#5531=DIRECTION('ref_axis',(0.,0.,-1.));
#5532=DIRECTION('center_axis',(1.,0.,0.));
#5533=DIRECTION('ref_axis',(0.,0.,-1.));
#5534=DIRECTION('',(1.,0.,0.));
#5535=DIRECTION('center_axis',(-1.,0.,0.));
#5536=DIRECTION('ref_axis',(0.,0.,-1.));
#5537=DIRECTION('center_axis',(1.,0.,0.));
#5538=DIRECTION('ref_axis',(0.,0.,-1.));
#5539=DIRECTION('',(1.,0.,0.));
#5540=DIRECTION('center_axis',(-1.,0.,0.));
#5541=DIRECTION('ref_axis',(0.,0.,-1.));
#5542=DIRECTION('center_axis',(0.,0.,1.));
#5543=DIRECTION('ref_axis',(1.,0.,0.));
#5544=DIRECTION('center_axis',(0.,0.,1.));
#5545=DIRECTION('ref_axis',(1.,0.,0.));
#5546=DIRECTION('',(0.,0.,1.));
#5547=DIRECTION('center_axis',(0.,0.,1.));
#5548=DIRECTION('ref_axis',(1.,0.,0.));
#5549=DIRECTION('center_axis',(0.,0.,1.));
#5550=DIRECTION('ref_axis',(1.,0.,0.));
#5551=DIRECTION('',(0.,0.,1.));
#5552=DIRECTION('center_axis',(0.,1.,0.));
#5553=DIRECTION('ref_axis',(1.,0.,0.));
#5554=DIRECTION('center_axis',(0.,1.,0.));
#5555=DIRECTION('ref_axis',(1.,0.,0.));
#5556=DIRECTION('',(0.,1.,0.));
#5557=DIRECTION('center_axis',(0.,-1.,0.));
#5558=DIRECTION('ref_axis',(1.,0.,0.));
#5559=DIRECTION('center_axis',(0.,-1.,0.));
#5560=DIRECTION('ref_axis',(0.,0.,-1.));
#5561=DIRECTION('',(0.,0.,-1.));
#5562=DIRECTION('',(1.,0.,0.));
#5563=DIRECTION('',(0.,0.,1.));
#5564=DIRECTION('',(0.,0.,1.));
#5565=DIRECTION('',(-1.,0.,0.));
#5566=DIRECTION('',(0.,0.,-1.));
#5567=DIRECTION('',(-1.,0.,0.));
#5568=DIRECTION('',(0.,0.,1.));
#5569=DIRECTION('',(-1.,0.,0.));
#5570=DIRECTION('center_axis',(-1.,0.,0.));
#5571=DIRECTION('ref_axis',(0.,0.,1.));
#5572=DIRECTION('',(0.,0.,1.));
#5573=DIRECTION('',(0.,1.,0.));
#5574=DIRECTION('center_axis',(0.,0.,-1.));
#5575=DIRECTION('ref_axis',(-1.,0.,0.));
#5576=DIRECTION('',(-1.,0.,0.));
#5577=DIRECTION('',(0.,1.,0.));
#5578=DIRECTION('center_axis',(1.,0.,0.));
#5579=DIRECTION('ref_axis',(0.,0.,-1.));
#5580=DIRECTION('',(0.,0.,-1.));
#5581=DIRECTION('center_axis',(1.,0.,0.));
#5582=DIRECTION('ref_axis',(0.,0.,-1.));
#5583=DIRECTION('',(0.,0.,-1.));
#5584=DIRECTION('',(0.,1.,0.));
#5585=DIRECTION('center_axis',(0.,0.,1.));
#5586=DIRECTION('ref_axis',(1.,0.,0.));
#5587=DIRECTION('',(1.,0.,0.));
#5588=DIRECTION('',(0.,1.,0.));
#5589=DIRECTION('center_axis',(-1.,0.,0.));
#5590=DIRECTION('ref_axis',(0.,0.,1.));
#5591=DIRECTION('',(0.,0.,1.));
#5592=DIRECTION('',(0.,1.,0.));
#5593=DIRECTION('center_axis',(0.,0.,1.));
#5594=DIRECTION('ref_axis',(1.,0.,0.));
#5595=DIRECTION('',(1.,0.,0.));
#5596=DIRECTION('',(0.,1.,0.));
#5597=DIRECTION('center_axis',(1.,0.,0.));
#5598=DIRECTION('ref_axis',(0.,0.,-1.));
#5599=DIRECTION('',(0.,0.,-1.));
#5600=DIRECTION('',(0.,1.,0.));
#5601=DIRECTION('center_axis',(0.,0.,1.));
#5602=DIRECTION('ref_axis',(1.,0.,0.));
#5603=DIRECTION('',(1.,0.,0.));
#5604=DIRECTION('center_axis',(0.,1.,0.));
#5605=DIRECTION('ref_axis',(0.,0.,1.));
#5606=DIRECTION('axis',(0.,0.,1.));
#5607=DIRECTION('refdir',(1.,0.,0.));
#5608=DIRECTION('center_axis',(0.866025403784439,0.,-0.5));
#5609=DIRECTION('ref_axis',(0.5,0.,0.866025403784439));
#5610=DIRECTION('',(-0.5,0.,-0.866025403784439));
#5611=DIRECTION('',(0.,-1.,0.));
#5612=DIRECTION('',(0.5,0.,0.866025403784439));
#5613=DIRECTION('',(0.,-1.,0.));
#5614=DIRECTION('center_axis',(1.20185167898973E-16,0.,-1.));
#5615=DIRECTION('ref_axis',(1.,0.,1.20185167898973E-16));
#5616=DIRECTION('',(-1.,0.,-1.20185167898973E-16));
#5617=DIRECTION('',(0.,-1.,0.));
#5618=DIRECTION('',(1.,0.,1.20185167898973E-16));
#5619=DIRECTION('center_axis',(-0.866025403784439,0.,-0.5));
#5620=DIRECTION('ref_axis',(0.5,0.,-0.866025403784439));
#5621=DIRECTION('',(-0.5,0.,0.866025403784439));
#5622=DIRECTION('',(0.,-1.,0.));
#5623=DIRECTION('',(0.5,0.,-0.866025403784439));
#5624=DIRECTION('center_axis',(-0.866025403784439,0.,0.5));
#5625=DIRECTION('ref_axis',(-0.5,0.,-0.866025403784439));
#5626=DIRECTION('',(0.5,0.,0.866025403784439));
#5627=DIRECTION('',(0.,-1.,0.));
#5628=DIRECTION('',(-0.5,0.,-0.866025403784439));
#5629=DIRECTION('center_axis',(-2.40370335797945E-16,0.,1.));
#5630=DIRECTION('ref_axis',(-1.,0.,-2.40370335797945E-16));
#5631=DIRECTION('',(1.,0.,2.40370335797945E-16));
#5632=DIRECTION('',(0.,-1.,0.));
#5633=DIRECTION('',(-1.,0.,-2.40370335797945E-16));
#5634=DIRECTION('center_axis',(0.866025403784439,0.,0.5));
#5635=DIRECTION('ref_axis',(-0.5,0.,0.866025403784439));
#5636=DIRECTION('',(0.5,0.,-0.866025403784439));
#5637=DIRECTION('',(-0.5,0.,0.866025403784439));
#5638=DIRECTION('center_axis',(0.,1.,0.));
#5639=DIRECTION('ref_axis',(1.,0.,0.));
#5640=DIRECTION('center_axis',(0.,-1.,0.));
#5641=DIRECTION('ref_axis',(0.,0.,-1.));
#5642=DIRECTION('center_axis',(0.,1.,0.));
#5643=DIRECTION('ref_axis',(1.,0.,0.));
#5644=DIRECTION('center_axis',(0.,1.,0.));
#5645=DIRECTION('ref_axis',(1.,0.,0.));
#5646=DIRECTION('center_axis',(0.,1.,0.));
#5647=DIRECTION('ref_axis',(0.,0.,1.));
#5648=DIRECTION('center_axis',(0.,-1.,0.));
#5649=DIRECTION('ref_axis',(1.,0.,0.));
#5650=DIRECTION('center_axis',(0.,-1.,0.));
#5651=DIRECTION('ref_axis',(1.,0.,0.));
#5652=DIRECTION('center_axis',(0.,-1.,0.));
#5653=DIRECTION('ref_axis',(1.,0.,0.));
#5654=DIRECTION('',(0.707106781186548,0.707106781186547,8.65956056235493E-17));
#5655=DIRECTION('center_axis',(0.,-1.,0.));
#5656=DIRECTION('ref_axis',(1.,0.,0.));
#5657=DIRECTION('center_axis',(0.,-1.,0.));
#5658=DIRECTION('ref_axis',(1.,0.,0.));
#5659=DIRECTION('',(0.,1.,0.));
#5660=DIRECTION('center_axis',(0.,1.,0.));
#5661=DIRECTION('ref_axis',(1.,0.,0.));
#5662=DIRECTION('center_axis',(0.,-1.,0.));
#5663=DIRECTION('ref_axis',(1.,0.,0.));
#5664=DIRECTION('',(-0.707106781186547,0.707106781186548,-8.65956056235493E-17));
#5665=DIRECTION('center_axis',(0.,-1.,0.));
#5666=DIRECTION('ref_axis',(0.,0.,-1.));
#5667=DIRECTION('center_axis',(0.,-1.,0.));
#5668=DIRECTION('ref_axis',(1.,0.,0.));
#5669=DIRECTION('center_axis',(0.,1.,0.));
#5670=DIRECTION('ref_axis',(1.,0.,0.));
#5671=DIRECTION('center_axis',(0.,1.,0.));
#5672=DIRECTION('ref_axis',(1.,0.,0.));
#5673=DIRECTION('',(-0.447213595499958,0.894427190999916,-5.47678698264203E-17));
#5674=DIRECTION('center_axis',(0.,-1.,0.));
#5675=DIRECTION('ref_axis',(1.,0.,0.));
#5676=DIRECTION('',(0.,1.,0.));
#5677=DIRECTION('axis',(0.,0.,1.));
#5678=DIRECTION('refdir',(1.,0.,0.));
#5679=DIRECTION('axis',(0.,0.,1.));
#5680=DIRECTION('refdir',(1.,0.,0.));
#5681=DIRECTION('center_axis',(1.,0.,0.));
#5682=DIRECTION('ref_axis',(0.,0.,-1.));
#5683=DIRECTION('center_axis',(1.,0.,0.));
#5684=DIRECTION('ref_axis',(0.,0.,-1.));
#5685=DIRECTION('',(1.,0.,0.));
#5686=DIRECTION('center_axis',(-1.,0.,0.));
#5687=DIRECTION('ref_axis',(0.,0.,-1.));
#5688=DIRECTION('center_axis',(1.,0.,0.));
#5689=DIRECTION('ref_axis',(0.,0.,-1.));
#5690=DIRECTION('center_axis',(1.,0.,0.));
#5691=DIRECTION('ref_axis',(0.,0.,-1.));
#5692=DIRECTION('center_axis',(1.,0.,0.));
#5693=DIRECTION('ref_axis',(0.,0.,-1.));
#5694=DIRECTION('',(1.,0.,0.));
#5695=DIRECTION('center_axis',(-1.,0.,0.));
#5696=DIRECTION('ref_axis',(0.,0.,-1.));
#5697=DIRECTION('center_axis',(1.,0.,0.));
#5698=DIRECTION('ref_axis',(0.,0.,-1.));
#5699=DIRECTION('center_axis',(1.,0.,0.));
#5700=DIRECTION('ref_axis',(0.,0.,-1.));
#5701=DIRECTION('center_axis',(1.,0.,0.));
#5702=DIRECTION('ref_axis',(0.,0.,-1.));
#5703=DIRECTION('',(1.,0.,0.));
#5704=DIRECTION('center_axis',(-1.,0.,0.));
#5705=DIRECTION('ref_axis',(0.,0.,-1.));
#5706=DIRECTION('center_axis',(1.,0.,0.));
#5707=DIRECTION('ref_axis',(0.,0.,-1.));
#5708=DIRECTION('center_axis',(1.,0.,0.));
#5709=DIRECTION('ref_axis',(0.,0.,-1.));
#5710=DIRECTION('center_axis',(1.,0.,0.));
#5711=DIRECTION('ref_axis',(0.,0.,-1.));
#5712=DIRECTION('',(1.,0.,0.));
#5713=DIRECTION('center_axis',(-1.,0.,0.));
#5714=DIRECTION('ref_axis',(0.,0.,-1.));
#5715=DIRECTION('center_axis',(1.,0.,0.));
#5716=DIRECTION('ref_axis',(0.,0.,-1.));
#5717=DIRECTION('center_axis',(1.,0.,0.));
#5718=DIRECTION('ref_axis',(0.,0.,-1.));
#5719=DIRECTION('center_axis',(1.,0.,0.));
#5720=DIRECTION('ref_axis',(0.,0.,-1.));
#5721=DIRECTION('',(1.,0.,0.));
#5722=DIRECTION('center_axis',(1.,0.,0.));
#5723=DIRECTION('ref_axis',(0.,0.,-1.));
#5724=DIRECTION('center_axis',(1.,0.,0.));
#5725=DIRECTION('ref_axis',(0.,0.,-1.));
#5726=DIRECTION('center_axis',(1.,0.,0.));
#5727=DIRECTION('ref_axis',(0.,0.,-1.));
#5728=DIRECTION('center_axis',(1.,0.,0.));
#5729=DIRECTION('ref_axis',(0.,0.,-1.));
#5730=DIRECTION('',(1.,0.,0.));
#5731=DIRECTION('center_axis',(1.,0.,0.));
#5732=DIRECTION('ref_axis',(0.,0.,-1.));
#5733=DIRECTION('center_axis',(1.,0.,0.));
#5734=DIRECTION('ref_axis',(0.,0.,-1.));
#5735=DIRECTION('center_axis',(1.,0.,0.));
#5736=DIRECTION('ref_axis',(0.,0.,-1.));
#5737=DIRECTION('center_axis',(1.,0.,0.));
#5738=DIRECTION('ref_axis',(0.,0.,-1.));
#5739=DIRECTION('',(1.,0.,0.));
#5740=DIRECTION('center_axis',(1.,0.,0.));
#5741=DIRECTION('ref_axis',(0.,0.,-1.));
#5742=DIRECTION('center_axis',(1.,0.,0.));
#5743=DIRECTION('ref_axis',(0.,0.,-1.));
#5744=DIRECTION('center_axis',(1.,0.,0.));
#5745=DIRECTION('ref_axis',(0.,0.,-1.));
#5746=DIRECTION('center_axis',(1.,0.,0.));
#5747=DIRECTION('ref_axis',(0.,0.,-1.));
#5748=DIRECTION('',(1.,0.,0.));
#5749=DIRECTION('center_axis',(1.,0.,0.));
#5750=DIRECTION('ref_axis',(0.,0.,-1.));
#5751=DIRECTION('center_axis',(1.,0.,0.));
#5752=DIRECTION('ref_axis',(0.,0.,-1.));
#5753=DIRECTION('center_axis',(0.,0.,1.));
#5754=DIRECTION('ref_axis',(1.,0.,0.));
#5755=DIRECTION('center_axis',(0.,0.,1.));
#5756=DIRECTION('ref_axis',(1.,0.,0.));
#5757=DIRECTION('',(0.,0.,1.));
#5758=DIRECTION('center_axis',(0.,0.,-1.));
#5759=DIRECTION('ref_axis',(1.,0.,0.));
#5760=DIRECTION('center_axis',(0.,0.,1.));
#5761=DIRECTION('ref_axis',(1.,0.,0.));
#5762=DIRECTION('center_axis',(0.,0.,1.));
#5763=DIRECTION('ref_axis',(1.,0.,0.));
#5764=DIRECTION('center_axis',(0.,0.,1.));
#5765=DIRECTION('ref_axis',(1.,0.,0.));
#5766=DIRECTION('',(0.,0.,1.));
#5767=DIRECTION('center_axis',(0.,0.,-1.));
#5768=DIRECTION('ref_axis',(1.,0.,0.));
#5769=DIRECTION('center_axis',(0.,0.,1.));
#5770=DIRECTION('ref_axis',(1.,0.,0.));
#5771=DIRECTION('center_axis',(0.,0.,1.));
#5772=DIRECTION('ref_axis',(1.,0.,0.));
#5773=DIRECTION('center_axis',(0.,0.,1.));
#5774=DIRECTION('ref_axis',(1.,0.,0.));
#5775=DIRECTION('',(0.,0.,1.));
#5776=DIRECTION('center_axis',(0.,0.,-1.));
#5777=DIRECTION('ref_axis',(1.,0.,0.));
#5778=DIRECTION('center_axis',(0.,0.,1.));
#5779=DIRECTION('ref_axis',(1.,0.,0.));
#5780=DIRECTION('center_axis',(0.,0.,1.));
#5781=DIRECTION('ref_axis',(1.,0.,0.));
#5782=DIRECTION('center_axis',(0.,0.,1.));
#5783=DIRECTION('ref_axis',(1.,0.,0.));
#5784=DIRECTION('',(0.,0.,1.));
#5785=DIRECTION('center_axis',(0.,0.,-1.));
#5786=DIRECTION('ref_axis',(1.,0.,0.));
#5787=DIRECTION('center_axis',(0.,0.,1.));
#5788=DIRECTION('ref_axis',(1.,0.,0.));
#5789=DIRECTION('center_axis',(1.,0.,0.));
#5790=DIRECTION('ref_axis',(0.,0.,-1.));
#5791=DIRECTION('center_axis',(1.,0.,0.));
#5792=DIRECTION('ref_axis',(0.,0.,-1.));
#5793=DIRECTION('',(1.,0.,0.));
#5794=DIRECTION('center_axis',(-1.,0.,0.));
#5795=DIRECTION('ref_axis',(0.,0.,-1.));
#5796=DIRECTION('center_axis',(1.,0.,0.));
#5797=DIRECTION('ref_axis',(0.,0.,-1.));
#5798=DIRECTION('center_axis',(1.,0.,0.));
#5799=DIRECTION('ref_axis',(0.,0.,-1.));
#5800=DIRECTION('',(1.,0.,0.));
#5801=DIRECTION('center_axis',(-1.,0.,0.));
#5802=DIRECTION('ref_axis',(0.,0.,-1.));
#5803=DIRECTION('center_axis',(0.,1.,0.));
#5804=DIRECTION('ref_axis',(-1.,0.,0.));
#5805=DIRECTION('',(-1.,0.,0.));
#5806=DIRECTION('',(0.,0.,1.));
#5807=DIRECTION('',(-1.,0.,0.));
#5808=DIRECTION('',(0.,0.,1.));
#5809=DIRECTION('center_axis',(1.,0.,0.));
#5810=DIRECTION('ref_axis',(0.,1.,0.));
#5811=DIRECTION('',(0.,1.,0.));
#5812=DIRECTION('',(0.,1.,0.));
#5813=DIRECTION('',(0.,0.,1.));
#5814=DIRECTION('center_axis',(0.,-1.,0.));
#5815=DIRECTION('ref_axis',(1.,0.,0.));
#5816=DIRECTION('',(1.,0.,0.));
#5817=DIRECTION('',(1.,0.,0.));
#5818=DIRECTION('',(0.,0.,1.));
#5819=DIRECTION('center_axis',(-1.,0.,0.));
#5820=DIRECTION('ref_axis',(0.,-1.,0.));
#5821=DIRECTION('',(0.,-1.,0.));
#5822=DIRECTION('',(0.,-1.,0.));
#5823=DIRECTION('center_axis',(0.,0.,1.));
#5824=DIRECTION('ref_axis',(1.,0.,0.));
#5825=DIRECTION('center_axis',(0.,0.,1.));
#5826=DIRECTION('ref_axis',(1.,0.,0.));
#5827=DIRECTION('axis',(0.,0.,1.));
#5828=DIRECTION('refdir',(1.,0.,0.));
#5829=DIRECTION('center_axis',(1.,0.,0.));
#5830=DIRECTION('ref_axis',(0.,0.,-1.));
#5831=DIRECTION('center_axis',(-1.,0.,0.));
#5832=DIRECTION('ref_axis',(0.,0.,-1.));
#5833=DIRECTION('',(-1.,0.,0.));
#5834=DIRECTION('center_axis',(-1.,0.,0.));
#5835=DIRECTION('ref_axis',(0.,0.,-1.));
#5836=DIRECTION('center_axis',(1.,0.,0.));
#5837=DIRECTION('ref_axis',(0.,0.,-1.));
#5838=DIRECTION('center_axis',(1.,0.,0.));
#5839=DIRECTION('ref_axis',(0.,0.,-1.));
#5840=DIRECTION('',(-1.,0.,0.));
#5841=DIRECTION('center_axis',(1.,0.,0.));
#5842=DIRECTION('ref_axis',(0.,0.,-1.));
#5843=DIRECTION('center_axis',(1.,0.,0.));
#5844=DIRECTION('ref_axis',(0.,0.,-1.));
#5845=DIRECTION('center_axis',(1.,0.,0.));
#5846=DIRECTION('ref_axis',(0.,0.,-1.));
#5847=DIRECTION('axis',(0.,0.,1.));
#5848=DIRECTION('refdir',(1.,0.,0.));
#5849=DIRECTION('center_axis',(1.,0.,0.));
#5850=DIRECTION('ref_axis',(0.,0.,-1.));
#5851=DIRECTION('center_axis',(-1.,0.,0.));
#5852=DIRECTION('ref_axis',(0.,0.,-1.));
#5853=DIRECTION('',(-1.,0.,0.));
#5854=DIRECTION('center_axis',(-1.,0.,0.));
#5855=DIRECTION('ref_axis',(0.,0.,-1.));
#5856=DIRECTION('center_axis',(1.,0.,0.));
#5857=DIRECTION('ref_axis',(0.,0.,-1.));
#5858=DIRECTION('center_axis',(1.,0.,0.));
#5859=DIRECTION('ref_axis',(0.,0.,-1.));
#5860=DIRECTION('',(-1.,0.,0.));
#5861=DIRECTION('center_axis',(1.,0.,0.));
#5862=DIRECTION('ref_axis',(0.,0.,-1.));
#5863=DIRECTION('center_axis',(1.,0.,0.));
#5864=DIRECTION('ref_axis',(0.,0.,-1.));
#5865=DIRECTION('center_axis',(1.,0.,0.));
#5866=DIRECTION('ref_axis',(0.,0.,-1.));
#5867=DIRECTION('axis',(0.,0.,1.));
#5868=DIRECTION('refdir',(1.,0.,0.));
#5869=DIRECTION('center_axis',(1.,0.,0.));
#5870=DIRECTION('ref_axis',(0.,0.,-1.));
#5871=DIRECTION('center_axis',(1.,0.,0.));
#5872=DIRECTION('ref_axis',(0.,0.,-1.));
#5873=DIRECTION('',(1.,0.,0.));
#5874=DIRECTION('center_axis',(-1.,0.,0.));
#5875=DIRECTION('ref_axis',(0.,0.,-1.));
#5876=DIRECTION('center_axis',(1.,0.,0.));
#5877=DIRECTION('ref_axis',(0.,0.,-1.));
#5878=DIRECTION('center_axis',(1.,0.,0.));
#5879=DIRECTION('ref_axis',(0.,0.,-1.));
#5880=DIRECTION('',(1.,0.,0.));
#5881=DIRECTION('center_axis',(-1.,0.,0.));
#5882=DIRECTION('ref_axis',(0.,0.,-1.));
#5883=DIRECTION('center_axis',(1.,0.,0.));
#5884=DIRECTION('ref_axis',(0.,0.,-1.));
#5885=DIRECTION('center_axis',(1.,0.,0.));
#5886=DIRECTION('ref_axis',(0.,0.,-1.));
#5887=DIRECTION('',(1.,0.,0.));
#5888=DIRECTION('center_axis',(-1.,0.,0.));
#5889=DIRECTION('ref_axis',(0.,0.,-1.));
#5890=DIRECTION('center_axis',(1.,0.,0.));
#5891=DIRECTION('ref_axis',(0.,0.,-1.));
#5892=DIRECTION('center_axis',(1.,0.,0.));
#5893=DIRECTION('ref_axis',(0.,0.,-1.));
#5894=DIRECTION('',(1.,0.,0.));
#5895=DIRECTION('center_axis',(-1.,0.,0.));
#5896=DIRECTION('ref_axis',(0.,0.,-1.));
#5897=DIRECTION('center_axis',(1.,0.,0.));
#5898=DIRECTION('ref_axis',(0.,0.,-1.));
#5899=DIRECTION('center_axis',(1.,0.,0.));
#5900=DIRECTION('ref_axis',(0.,0.,-1.));
#5901=DIRECTION('',(1.,0.,0.));
#5902=DIRECTION('center_axis',(-1.,0.,0.));
#5903=DIRECTION('ref_axis',(0.,0.,-1.));
#5904=DIRECTION('center_axis',(1.,0.,0.));
#5905=DIRECTION('ref_axis',(0.,0.,-1.));
#5906=DIRECTION('center_axis',(1.,0.,0.));
#5907=DIRECTION('ref_axis',(0.,0.,-1.));
#5908=DIRECTION('',(1.,0.,0.));
#5909=DIRECTION('center_axis',(-1.,0.,0.));
#5910=DIRECTION('ref_axis',(0.,0.,-1.));
#5911=DIRECTION('center_axis',(0.,1.,0.));
#5912=DIRECTION('ref_axis',(-1.,0.,0.));
#5913=DIRECTION('',(-1.,0.,0.));
#5914=DIRECTION('',(0.,0.,1.));
#5915=DIRECTION('',(-1.,0.,0.));
#5916=DIRECTION('',(0.,0.,1.));
#5917=DIRECTION('center_axis',(1.,0.,0.));
#5918=DIRECTION('ref_axis',(0.,1.,0.));
#5919=DIRECTION('',(0.,1.,0.));
#5920=DIRECTION('',(0.,1.,0.));
#5921=DIRECTION('',(0.,0.,1.));
#5922=DIRECTION('center_axis',(0.,-1.,0.));
#5923=DIRECTION('ref_axis',(1.,0.,0.));
#5924=DIRECTION('',(1.,0.,0.));
#5925=DIRECTION('',(1.,0.,0.));
#5926=DIRECTION('',(0.,0.,1.));
#5927=DIRECTION('center_axis',(-1.,0.,0.));
#5928=DIRECTION('ref_axis',(0.,-1.,0.));
#5929=DIRECTION('',(0.,-1.,0.));
#5930=DIRECTION('',(0.,-1.,0.));
#5931=DIRECTION('center_axis',(0.,0.,1.));
#5932=DIRECTION('ref_axis',(1.,0.,0.));
#5933=DIRECTION('center_axis',(0.,0.,1.));
#5934=DIRECTION('ref_axis',(1.,0.,0.));
#5935=DIRECTION('axis',(0.,0.,1.));
#5936=DIRECTION('refdir',(1.,0.,0.));
#5937=DIRECTION('center_axis',(1.,0.,0.));
#5938=DIRECTION('ref_axis',(0.,0.,-1.));
#5939=DIRECTION('center_axis',(1.,0.,0.));
#5940=DIRECTION('ref_axis',(0.,0.,-1.));
#5941=DIRECTION('',(1.,0.,0.));
#5942=DIRECTION('center_axis',(-1.,0.,0.));
#5943=DIRECTION('ref_axis',(0.,0.,-1.));
#5944=DIRECTION('center_axis',(1.,0.,0.));
#5945=DIRECTION('ref_axis',(0.,0.,-1.));
#5946=DIRECTION('center_axis',(1.,0.,0.));
#5947=DIRECTION('ref_axis',(0.,0.,-1.));
#5948=DIRECTION('',(1.,0.,0.));
#5949=DIRECTION('center_axis',(-1.,0.,0.));
#5950=DIRECTION('ref_axis',(0.,0.,-1.));
#5951=DIRECTION('center_axis',(1.,0.,0.));
#5952=DIRECTION('ref_axis',(0.,0.,-1.));
#5953=DIRECTION('center_axis',(1.,0.,0.));
#5954=DIRECTION('ref_axis',(0.,0.,-1.));
#5955=DIRECTION('',(1.,0.,0.));
#5956=DIRECTION('center_axis',(-1.,0.,0.));
#5957=DIRECTION('ref_axis',(0.,0.,-1.));
#5958=DIRECTION('center_axis',(1.,0.,0.));
#5959=DIRECTION('ref_axis',(0.,0.,-1.));
#5960=DIRECTION('center_axis',(1.,0.,0.));
#5961=DIRECTION('ref_axis',(0.,0.,-1.));
#5962=DIRECTION('',(1.,0.,0.));
#5963=DIRECTION('center_axis',(-1.,0.,0.));
#5964=DIRECTION('ref_axis',(0.,0.,-1.));
#5965=DIRECTION('center_axis',(1.,0.,0.));
#5966=DIRECTION('ref_axis',(0.,0.,-1.));
#5967=DIRECTION('center_axis',(1.,0.,0.));
#5968=DIRECTION('ref_axis',(0.,0.,-1.));
#5969=DIRECTION('',(1.,0.,0.));
#5970=DIRECTION('center_axis',(-1.,0.,0.));
#5971=DIRECTION('ref_axis',(0.,0.,-1.));
#5972=DIRECTION('center_axis',(1.,0.,0.));
#5973=DIRECTION('ref_axis',(0.,0.,-1.));
#5974=DIRECTION('center_axis',(1.,0.,0.));
#5975=DIRECTION('ref_axis',(0.,0.,-1.));
#5976=DIRECTION('',(1.,0.,0.));
#5977=DIRECTION('center_axis',(-1.,0.,0.));
#5978=DIRECTION('ref_axis',(0.,0.,-1.));
#5979=DIRECTION('center_axis',(0.,1.,0.));
#5980=DIRECTION('ref_axis',(-1.,0.,0.));
#5981=DIRECTION('',(-1.,0.,0.));
#5982=DIRECTION('',(0.,0.,1.));
#5983=DIRECTION('',(-1.,0.,0.));
#5984=DIRECTION('',(0.,0.,1.));
#5985=DIRECTION('center_axis',(1.,0.,0.));
#5986=DIRECTION('ref_axis',(0.,1.,0.));
#5987=DIRECTION('',(0.,1.,0.));
#5988=DIRECTION('',(0.,1.,0.));
#5989=DIRECTION('',(0.,0.,1.));
#5990=DIRECTION('center_axis',(0.,-1.,0.));
#5991=DIRECTION('ref_axis',(1.,0.,0.));
#5992=DIRECTION('',(1.,0.,0.));
#5993=DIRECTION('',(1.,0.,0.));
#5994=DIRECTION('',(0.,0.,1.));
#5995=DIRECTION('center_axis',(-1.,0.,0.));
#5996=DIRECTION('ref_axis',(0.,-1.,0.));
#5997=DIRECTION('',(0.,-1.,0.));
#5998=DIRECTION('',(0.,-1.,0.));
#5999=DIRECTION('center_axis',(0.,0.,1.));
#6000=DIRECTION('ref_axis',(1.,0.,0.));
#6001=DIRECTION('center_axis',(0.,0.,1.));
#6002=DIRECTION('ref_axis',(1.,0.,0.));
#6003=DIRECTION('axis',(0.,0.,1.));
#6004=DIRECTION('refdir',(1.,0.,0.));
#6005=DIRECTION('center_axis',(0.,0.,1.));
#6006=DIRECTION('ref_axis',(1.,0.,0.));
#6007=DIRECTION('center_axis',(0.,0.,1.));
#6008=DIRECTION('ref_axis',(1.,0.,0.));
#6009=DIRECTION('',(0.,0.,1.));
#6010=DIRECTION('center_axis',(0.,0.,-1.));
#6011=DIRECTION('ref_axis',(1.,0.,0.));
#6012=DIRECTION('center_axis',(0.,0.,1.));
#6013=DIRECTION('ref_axis',(1.,0.,0.));
#6014=DIRECTION('center_axis',(0.,0.,1.));
#6015=DIRECTION('ref_axis',(1.,0.,0.));
#6016=DIRECTION('',(0.,0.,1.));
#6017=DIRECTION('center_axis',(0.,0.,-1.));
#6018=DIRECTION('ref_axis',(1.,0.,0.));
#6019=DIRECTION('center_axis',(0.,0.,1.));
#6020=DIRECTION('ref_axis',(1.,0.,0.));
#6021=DIRECTION('center_axis',(0.,0.,1.));
#6022=DIRECTION('ref_axis',(1.,0.,0.));
#6023=DIRECTION('',(0.,0.,1.));
#6024=DIRECTION('center_axis',(0.,0.,-1.));
#6025=DIRECTION('ref_axis',(1.,0.,0.));
#6026=DIRECTION('center_axis',(0.,0.,1.));
#6027=DIRECTION('ref_axis',(1.,0.,0.));
#6028=DIRECTION('center_axis',(0.,0.,1.));
#6029=DIRECTION('ref_axis',(1.,0.,0.));
#6030=DIRECTION('',(0.,0.,1.));
#6031=DIRECTION('center_axis',(0.,0.,-1.));
#6032=DIRECTION('ref_axis',(1.,0.,0.));
#6033=DIRECTION('center_axis',(0.,0.,1.));
#6034=DIRECTION('ref_axis',(1.,0.,0.));
#6035=DIRECTION('center_axis',(0.,0.,1.));
#6036=DIRECTION('ref_axis',(1.,0.,0.));
#6037=DIRECTION('',(0.,0.,1.));
#6038=DIRECTION('center_axis',(0.,0.,-1.));
#6039=DIRECTION('ref_axis',(1.,0.,0.));
#6040=DIRECTION('center_axis',(0.,1.,0.));
#6041=DIRECTION('ref_axis',(-1.,0.,0.));
#6042=DIRECTION('',(-1.,0.,0.));
#6043=DIRECTION('',(0.,0.,1.));
#6044=DIRECTION('',(-1.,0.,0.));
#6045=DIRECTION('',(0.,0.,1.));
#6046=DIRECTION('center_axis',(1.,0.,0.));
#6047=DIRECTION('ref_axis',(0.,1.,0.));
#6048=DIRECTION('',(0.,1.,0.));
#6049=DIRECTION('',(0.,1.,0.));
#6050=DIRECTION('',(0.,0.,1.));
#6051=DIRECTION('center_axis',(0.,-1.,0.));
#6052=DIRECTION('ref_axis',(1.,0.,0.));
#6053=DIRECTION('',(1.,0.,0.));
#6054=DIRECTION('',(1.,0.,0.));
#6055=DIRECTION('',(0.,0.,1.));
#6056=DIRECTION('center_axis',(-1.,0.,0.));
#6057=DIRECTION('ref_axis',(0.,-1.,0.));
#6058=DIRECTION('',(0.,-1.,0.));
#6059=DIRECTION('',(0.,-1.,0.));
#6060=DIRECTION('center_axis',(0.,0.,1.));
#6061=DIRECTION('ref_axis',(1.,0.,0.));
#6062=DIRECTION('center_axis',(0.,0.,1.));
#6063=DIRECTION('ref_axis',(1.,0.,0.));
#6064=DIRECTION('axis',(0.,0.,1.));
#6065=DIRECTION('refdir',(1.,0.,0.));
#6066=DIRECTION('center_axis',(0.,0.,1.));
#6067=DIRECTION('ref_axis',(1.,0.,0.));
#6068=DIRECTION('center_axis',(0.,0.,-1.));
#6069=DIRECTION('ref_axis',(1.,0.,0.));
#6070=DIRECTION('',(0.,0.,-1.));
#6071=DIRECTION('center_axis',(0.,0.,-1.));
#6072=DIRECTION('ref_axis',(1.,0.,0.));
#6073=DIRECTION('center_axis',(0.,0.,1.));
#6074=DIRECTION('ref_axis',(1.,0.,0.));
#6075=DIRECTION('center_axis',(0.,0.,1.));
#6076=DIRECTION('ref_axis',(1.,0.,0.));
#6077=DIRECTION('',(0.,0.,-1.));
#6078=DIRECTION('center_axis',(0.,0.,1.));
#6079=DIRECTION('ref_axis',(1.,0.,0.));
#6080=DIRECTION('center_axis',(0.,0.,1.));
#6081=DIRECTION('ref_axis',(1.,0.,0.));
#6082=DIRECTION('center_axis',(0.,0.,1.));
#6083=DIRECTION('ref_axis',(1.,0.,0.));
#6084=DIRECTION('axis',(0.,0.,1.));
#6085=DIRECTION('refdir',(1.,0.,0.));
#6086=DIRECTION('axis',(0.,0.,1.));
#6087=DIRECTION('refdir',(1.,0.,0.));
#6088=DIRECTION('center_axis',(0.,1.,0.));
#6089=DIRECTION('ref_axis',(0.,0.,1.));
#6090=DIRECTION('center_axis',(0.,-1.,0.));
#6091=DIRECTION('ref_axis',(1.,0.,0.));
#6092=DIRECTION('',(-1.,0.,0.));
#6093=DIRECTION('',(0.,0.,-1.));
#6094=DIRECTION('',(1.,0.,0.));
#6095=DIRECTION('center_axis',(0.,0.,1.));
#6096=DIRECTION('ref_axis',(1.,0.,0.));
#6097=DIRECTION('',(0.,-1.,0.));
#6098=DIRECTION('',(0.,1.,0.));
#6099=DIRECTION('',(-1.,0.,0.));
#6100=DIRECTION('center_axis',(0.,-1.,0.));
#6101=DIRECTION('ref_axis',(0.,0.,-1.));
#6102=DIRECTION('center_axis',(0.,1.,0.));
#6103=DIRECTION('ref_axis',(1.,0.,0.));
#6104=DIRECTION('',(0.,0.,1.));
#6105=DIRECTION('',(1.,0.,0.));
#6106=DIRECTION('center_axis',(0.,0.,-1.));
#6107=DIRECTION('ref_axis',(-1.,0.,0.));
#6108=DIRECTION('',(0.,1.,0.));
#6109=DIRECTION('',(0.,1.,0.));
#6110=DIRECTION('center_axis',(1.,0.,0.));
#6111=DIRECTION('ref_axis',(0.,0.,-1.));
#6112=DIRECTION('center_axis',(0.,1.,0.));
#6113=DIRECTION('ref_axis',(0.,0.,1.));
#6114=DIRECTION('center_axis',(0.,-1.,0.));
#6115=DIRECTION('ref_axis',(1.,0.,0.));
#6116=DIRECTION('center_axis',(0.,-1.,0.));
#6117=DIRECTION('ref_axis',(1.,0.,0.));
#6118=DIRECTION('center_axis',(0.,-1.,0.));
#6119=DIRECTION('ref_axis',(1.,0.,0.));
#6120=DIRECTION('center_axis',(0.,-1.,0.));
#6121=DIRECTION('ref_axis',(1.,0.,0.));
#6122=DIRECTION('',(0.,1.,0.));
#6123=DIRECTION('center_axis',(0.,-1.,0.));
#6124=DIRECTION('ref_axis',(0.,0.,-1.));
#6125=DIRECTION('center_axis',(0.,-1.,0.));
#6126=DIRECTION('ref_axis',(1.,0.,0.));
#6127=DIRECTION('center_axis',(0.,-1.,0.));
#6128=DIRECTION('ref_axis',(1.,0.,0.));
#6129=DIRECTION('center_axis',(0.,-1.,0.));
#6130=DIRECTION('ref_axis',(1.,0.,0.));
#6131=DIRECTION('',(0.,1.,0.));
#6132=DIRECTION('center_axis',(0.,1.,0.));
#6133=DIRECTION('ref_axis',(0.,0.,1.));
#6134=DIRECTION('center_axis',(0.,-1.,0.));
#6135=DIRECTION('ref_axis',(1.,0.,0.));
#6136=DIRECTION('center_axis',(0.,-1.,0.));
#6137=DIRECTION('ref_axis',(1.,0.,0.));
#6138=DIRECTION('center_axis',(0.,-1.,0.));
#6139=DIRECTION('ref_axis',(1.,0.,0.));
#6140=DIRECTION('',(0.,1.,0.));
#6141=DIRECTION('center_axis',(0.,-1.,0.));
#6142=DIRECTION('ref_axis',(0.,0.,-1.));
#6143=DIRECTION('center_axis',(0.,-1.,0.));
#6144=DIRECTION('ref_axis',(1.,0.,0.));
#6145=DIRECTION('center_axis',(0.,-1.,0.));
#6146=DIRECTION('ref_axis',(1.,0.,0.));
#6147=DIRECTION('center_axis',(0.,-1.,0.));
#6148=DIRECTION('ref_axis',(1.,0.,0.));
#6149=DIRECTION('',(0.,1.,0.));
#6150=DIRECTION('center_axis',(0.,1.,0.));
#6151=DIRECTION('ref_axis',(0.,0.,1.));
#6152=DIRECTION('center_axis',(0.,-1.,0.));
#6153=DIRECTION('ref_axis',(1.,0.,0.));
#6154=DIRECTION('center_axis',(0.,-1.,0.));
#6155=DIRECTION('ref_axis',(1.,0.,0.));
#6156=DIRECTION('center_axis',(0.,-1.,0.));
#6157=DIRECTION('ref_axis',(1.,0.,0.));
#6158=DIRECTION('',(0.,1.,0.));
#6159=DIRECTION('center_axis',(0.,-1.,0.));
#6160=DIRECTION('ref_axis',(0.,0.,-1.));
#6161=DIRECTION('center_axis',(0.,-1.,0.));
#6162=DIRECTION('ref_axis',(1.,0.,0.));
#6163=DIRECTION('center_axis',(0.,-1.,0.));
#6164=DIRECTION('ref_axis',(1.,0.,0.));
#6165=DIRECTION('',(0.,1.,0.));
#6166=DIRECTION('axis',(0.,0.,1.));
#6167=DIRECTION('refdir',(1.,0.,0.));
#6168=DIRECTION('center_axis',(0.,1.,0.));
#6169=DIRECTION('ref_axis',(0.,0.,1.));
#6170=DIRECTION('center_axis',(0.,1.,0.));
#6171=DIRECTION('ref_axis',(1.,0.,0.));
#6172=DIRECTION('',(1.,0.,0.));
#6173=DIRECTION('center_axis',(0.,-1.,0.));
#6174=DIRECTION('ref_axis',(1.,0.,0.));
#6175=DIRECTION('',(-1.,0.,0.));
#6176=DIRECTION('center_axis',(0.,0.,-1.));
#6177=DIRECTION('ref_axis',(-1.,0.,0.));
#6178=DIRECTION('',(0.,-1.,0.));
#6179=DIRECTION('',(0.,1.,0.));
#6180=DIRECTION('',(1.,0.,0.));
#6181=DIRECTION('center_axis',(0.,-1.,0.));
#6182=DIRECTION('ref_axis',(0.,0.,-1.));
#6183=DIRECTION('center_axis',(0.,-1.,0.));
#6184=DIRECTION('ref_axis',(1.,0.,0.));
#6185=DIRECTION('center_axis',(0.,1.,0.));
#6186=DIRECTION('ref_axis',(1.,0.,0.));
#6187=DIRECTION('',(-1.,0.,0.));
#6188=DIRECTION('center_axis',(0.,0.,1.));
#6189=DIRECTION('ref_axis',(1.,0.,0.));
#6190=DIRECTION('',(0.,1.,0.));
#6191=DIRECTION('',(0.,-1.,0.));
#6192=DIRECTION('center_axis',(0.,1.,0.));
#6193=DIRECTION('ref_axis',(0.,0.,1.));
#6194=DIRECTION('center_axis',(0.,-1.,0.));
#6195=DIRECTION('ref_axis',(1.,0.,0.));
#6196=DIRECTION('center_axis',(0.,-1.,0.));
#6197=DIRECTION('ref_axis',(1.,0.,0.));
#6198=DIRECTION('center_axis',(0.,-1.,0.));
#6199=DIRECTION('ref_axis',(1.,0.,0.));
#6200=DIRECTION('center_axis',(0.,-1.,0.));
#6201=DIRECTION('ref_axis',(1.,0.,0.));
#6202=DIRECTION('',(0.,1.,0.));
#6203=DIRECTION('center_axis',(0.,-1.,0.));
#6204=DIRECTION('ref_axis',(0.,0.,-1.));
#6205=DIRECTION('center_axis',(0.,-1.,0.));
#6206=DIRECTION('ref_axis',(1.,0.,0.));
#6207=DIRECTION('center_axis',(0.,-1.,0.));
#6208=DIRECTION('ref_axis',(1.,0.,0.));
#6209=DIRECTION('',(0.,1.,0.));
#6210=DIRECTION('',(0.,0.,1.));
#6211=DIRECTION('',(1.,0.,0.));
#6212=DIRECTION('',(0.,0.,1.));
#6213=DIRECTION('',(1.,0.,0.));
#6214=DIRECTION('axis',(0.,0.,1.));
#6215=DIRECTION('refdir',(1.,0.,0.));
#6216=DIRECTION('center_axis',(0.,1.,0.));
#6217=DIRECTION('ref_axis',(0.,0.,1.));
#6218=DIRECTION('center_axis',(0.,-1.,0.));
#6219=DIRECTION('ref_axis',(1.,0.,0.));
#6220=DIRECTION('center_axis',(0.,-1.,0.));
#6221=DIRECTION('ref_axis',(1.,0.,0.));
#6222=DIRECTION('center_axis',(0.,-1.,0.));
#6223=DIRECTION('ref_axis',(1.,0.,0.));
#6224=DIRECTION('',(0.707106781186547,0.707106781186548,8.65956056235493E-17));
#6225=DIRECTION('center_axis',(0.,-1.,0.));
#6226=DIRECTION('ref_axis',(1.,0.,0.));
#6227=DIRECTION('center_axis',(0.,-1.,0.));
#6228=DIRECTION('ref_axis',(1.,0.,0.));
#6229=DIRECTION('',(0.,1.,0.));
#6230=DIRECTION('center_axis',(0.,1.,0.));
#6231=DIRECTION('ref_axis',(1.,0.,0.));
#6232=DIRECTION('center_axis',(0.,-1.,0.));
#6233=DIRECTION('ref_axis',(1.,0.,0.));
#6234=DIRECTION('',(-0.707106781186547,0.707106781186548,-8.65956056235493E-17));
#6235=DIRECTION('center_axis',(0.,-1.,0.));
#6236=DIRECTION('ref_axis',(0.,0.,-1.));
#6237=DIRECTION('center_axis',(0.,-1.,0.));
#6238=DIRECTION('ref_axis',(1.,0.,0.));
#6239=DIRECTION('center_axis',(0.,1.,0.));
#6240=DIRECTION('ref_axis',(1.,0.,0.));
#6241=DIRECTION('center_axis',(0.,1.,0.));
#6242=DIRECTION('ref_axis',(1.,0.,0.));
#6243=DIRECTION('',(-0.447213595499958,0.894427190999916,-5.47678698264203E-17));
#6244=DIRECTION('center_axis',(0.,-1.,0.));
#6245=DIRECTION('ref_axis',(1.,0.,0.));
#6246=DIRECTION('center_axis',(0.,1.,0.));
#6247=DIRECTION('ref_axis',(1.,0.,0.));
#6248=DIRECTION('',(0.,1.,0.));
#6249=DIRECTION('center_axis',(0.,1.,0.));
#6250=DIRECTION('ref_axis',(1.,0.,0.));
#6251=DIRECTION('center_axis',(0.,-1.,0.));
#6252=DIRECTION('ref_axis',(1.,0.,0.));
#6253=DIRECTION('',(-0.707106781186547,0.707106781186548,-8.65956056235493E-17));
#6254=DIRECTION('center_axis',(0.,-1.,0.));
#6255=DIRECTION('ref_axis',(0.,0.,-1.));
#6256=DIRECTION('center_axis',(0.866025403784439,0.,-0.5));
#6257=DIRECTION('ref_axis',(0.5,0.,0.866025403784439));
#6258=DIRECTION('',(-0.5,0.,-0.866025403784439));
#6259=DIRECTION('',(0.,-1.,0.));
#6260=DIRECTION('',(0.5,0.,0.866025403784439));
#6261=DIRECTION('',(0.,-1.,0.));
#6262=DIRECTION('center_axis',(1.60246890531964E-16,0.,-1.));
#6263=DIRECTION('ref_axis',(1.,0.,1.60246890531964E-16));
#6264=DIRECTION('',(-1.,0.,-1.60246890531964E-16));
#6265=DIRECTION('',(0.,-1.,0.));
#6266=DIRECTION('',(1.,0.,1.60246890531964E-16));
#6267=DIRECTION('center_axis',(-0.866025403784439,0.,-0.5));
#6268=DIRECTION('ref_axis',(0.5,0.,-0.866025403784439));
#6269=DIRECTION('',(-0.5,0.,0.866025403784439));
#6270=DIRECTION('',(0.,-1.,0.));
#6271=DIRECTION('',(0.5,0.,-0.866025403784439));
#6272=DIRECTION('center_axis',(-0.866025403784439,0.,0.5));
#6273=DIRECTION('ref_axis',(-0.5,0.,-0.866025403784439));
#6274=DIRECTION('',(0.5,0.,0.866025403784439));
#6275=DIRECTION('',(0.,-1.,0.));
#6276=DIRECTION('',(-0.5,0.,-0.866025403784439));
#6277=DIRECTION('center_axis',(-1.60246890531964E-16,0.,1.));
#6278=DIRECTION('ref_axis',(-1.,0.,-1.60246890531964E-16));
#6279=DIRECTION('',(1.,0.,1.60246890531964E-16));
#6280=DIRECTION('',(0.,-1.,0.));
#6281=DIRECTION('',(-1.,0.,-1.60246890531964E-16));
#6282=DIRECTION('center_axis',(0.866025403784439,0.,0.5));
#6283=DIRECTION('ref_axis',(-0.5,0.,0.866025403784439));
#6284=DIRECTION('',(0.5,0.,-0.866025403784439));
#6285=DIRECTION('',(-0.5,0.,0.866025403784439));
#6286=DIRECTION('center_axis',(0.,1.,0.));
#6287=DIRECTION('ref_axis',(1.,0.,0.));
#6288=DIRECTION('center_axis',(0.,-1.,0.));
#6289=DIRECTION('ref_axis',(0.,0.,-1.));
#6290=DIRECTION('axis',(0.,0.,1.));
#6291=DIRECTION('refdir',(1.,0.,0.));
#6292=DIRECTION('center_axis',(0.,1.,0.));
#6293=DIRECTION('ref_axis',(0.,0.,1.));
#6294=DIRECTION('center_axis',(0.,-1.,0.));
#6295=DIRECTION('ref_axis',(1.,0.,0.));
#6296=DIRECTION('center_axis',(0.,-1.,0.));
#6297=DIRECTION('ref_axis',(1.,0.,0.));
#6298=DIRECTION('center_axis',(0.,-1.,0.));
#6299=DIRECTION('ref_axis',(1.,0.,0.));
#6300=DIRECTION('',(0.707106781186548,0.707106781186547,8.65956056235493E-17));
#6301=DIRECTION('center_axis',(0.,-1.,0.));
#6302=DIRECTION('ref_axis',(1.,0.,0.));
#6303=DIRECTION('center_axis',(0.,-1.,0.));
#6304=DIRECTION('ref_axis',(1.,0.,0.));
#6305=DIRECTION('',(0.,1.,0.));
#6306=DIRECTION('center_axis',(0.,1.,0.));
#6307=DIRECTION('ref_axis',(1.,0.,0.));
#6308=DIRECTION('center_axis',(0.,-1.,0.));
#6309=DIRECTION('ref_axis',(1.,0.,0.));
#6310=DIRECTION('',(-0.707106781186547,0.707106781186548,-8.65956056235493E-17));
#6311=DIRECTION('center_axis',(0.,-1.,0.));
#6312=DIRECTION('ref_axis',(0.,0.,-1.));
#6313=DIRECTION('center_axis',(0.,-1.,0.));
#6314=DIRECTION('ref_axis',(1.,0.,0.));
#6315=DIRECTION('center_axis',(0.,1.,0.));
#6316=DIRECTION('ref_axis',(1.,0.,0.));
#6317=DIRECTION('center_axis',(0.,1.,0.));
#6318=DIRECTION('ref_axis',(1.,0.,0.));
#6319=DIRECTION('',(-0.447213595499958,0.894427190999916,-5.47678698264203E-17));
#6320=DIRECTION('center_axis',(0.,-1.,0.));
#6321=DIRECTION('ref_axis',(1.,0.,0.));
#6322=DIRECTION('center_axis',(0.,1.,0.));
#6323=DIRECTION('ref_axis',(1.,0.,0.));
#6324=DIRECTION('',(0.,1.,0.));
#6325=DIRECTION('center_axis',(0.,1.,0.));
#6326=DIRECTION('ref_axis',(1.,0.,0.));
#6327=DIRECTION('center_axis',(0.,-1.,0.));
#6328=DIRECTION('ref_axis',(1.,0.,0.));
#6329=DIRECTION('',(-0.707106781186547,0.707106781186548,-8.65956056235493E-17));
#6330=DIRECTION('center_axis',(0.,-1.,0.));
#6331=DIRECTION('ref_axis',(0.,0.,-1.));
#6332=DIRECTION('center_axis',(0.866025403784439,0.,-0.5));
#6333=DIRECTION('ref_axis',(0.5,0.,0.866025403784439));
#6334=DIRECTION('',(-0.5,0.,-0.866025403784439));
#6335=DIRECTION('',(0.,-1.,0.));
#6336=DIRECTION('',(0.5,0.,0.866025403784439));
#6337=DIRECTION('',(0.,-1.,0.));
#6338=DIRECTION('center_axis',(1.20185167898973E-16,0.,-1.));
#6339=DIRECTION('ref_axis',(1.,0.,1.20185167898973E-16));
#6340=DIRECTION('',(-1.,0.,-1.20185167898973E-16));
#6341=DIRECTION('',(0.,-1.,0.));
#6342=DIRECTION('',(1.,0.,1.20185167898973E-16));
#6343=DIRECTION('center_axis',(-0.866025403784439,0.,-0.5));
#6344=DIRECTION('ref_axis',(0.5,0.,-0.866025403784439));
#6345=DIRECTION('',(-0.5,0.,0.866025403784439));
#6346=DIRECTION('',(0.,-1.,0.));
#6347=DIRECTION('',(0.5,0.,-0.866025403784439));
#6348=DIRECTION('center_axis',(-0.866025403784439,0.,0.5));
#6349=DIRECTION('ref_axis',(-0.5,0.,-0.866025403784439));
#6350=DIRECTION('',(0.5,0.,0.866025403784439));
#6351=DIRECTION('',(0.,-1.,0.));
#6352=DIRECTION('',(-0.5,0.,-0.866025403784439));
#6353=DIRECTION('center_axis',(-2.40370335797945E-16,0.,1.));
#6354=DIRECTION('ref_axis',(-1.,0.,-2.40370335797945E-16));
#6355=DIRECTION('',(1.,0.,2.40370335797945E-16));
#6356=DIRECTION('',(0.,-1.,0.));
#6357=DIRECTION('',(-1.,0.,-2.40370335797945E-16));
#6358=DIRECTION('center_axis',(0.866025403784439,0.,0.5));
#6359=DIRECTION('ref_axis',(-0.5,0.,0.866025403784439));
#6360=DIRECTION('',(0.5,0.,-0.866025403784439));
#6361=DIRECTION('',(-0.5,0.,0.866025403784439));
#6362=DIRECTION('center_axis',(0.,1.,0.));
#6363=DIRECTION('ref_axis',(1.,0.,0.));
#6364=DIRECTION('center_axis',(0.,-1.,0.));
#6365=DIRECTION('ref_axis',(0.,0.,-1.));
#6366=DIRECTION('',(0.,0.,1.));
#6367=DIRECTION('',(1.,0.,0.));
#6368=DIRECTION('',(0.,0.,1.));
#6369=DIRECTION('',(1.,0.,0.));
#6370=DIRECTION('',(0.,0.,1.));
#6371=DIRECTION('',(1.,0.,0.));
#6372=DIRECTION('',(0.,0.,1.));
#6373=DIRECTION('',(1.,0.,0.));
#6374=DIRECTION('',(0.,0.,1.));
#6375=DIRECTION('',(1.,0.,0.));
#6376=DIRECTION('',(0.,0.,1.));
#6377=DIRECTION('',(1.,0.,0.));
#6378=DIRECTION('',(0.,0.,1.));
#6379=DIRECTION('',(2.22044604925031E-16,-1.,0.));
#6380=DIRECTION('',(0.,-1.,2.22044604925031E-16));
#6381=DIRECTION('',(1.,0.,0.));
#6382=DIRECTION('',(0.,-1.,2.22044604925031E-16));
#6383=DIRECTION('',(1.,0.,0.));
#6384=DIRECTION('',(0.,0.,1.));
#6385=DIRECTION('',(-1.,1.22464679914735E-16,0.));
#6386=DIRECTION('',(0.,0.,1.));
#6387=DIRECTION('',(2.22044604925031E-16,-1.,0.));
#6388=DIRECTION('',(0.,-1.,2.22044604925031E-16));
#6389=DIRECTION('',(1.,0.,0.));
#6390=DIRECTION('',(0.,-1.,2.22044604925031E-16));
#6391=DIRECTION('',(1.,0.,0.));
#6392=DIRECTION('',(0.,0.,1.));
#6393=DIRECTION('',(-1.,1.22464679914735E-16,0.));
#6394=DIRECTION('',(0.,0.,1.));
#6395=DIRECTION('',(1.,0.,0.));
#6396=DIRECTION('',(0.,0.,1.));
#6397=DIRECTION('',(2.22044604925031E-16,-1.,0.));
#6398=DIRECTION('',(0.,-1.,2.22044604925031E-16));
#6399=DIRECTION('',(1.,0.,0.));
#6400=DIRECTION('',(0.,-1.,2.22044604925031E-16));
#6401=DIRECTION('',(1.,0.,0.));
#6402=DIRECTION('',(0.,0.,1.));
#6403=DIRECTION('',(-1.,1.22464679914735E-16,0.));
#6404=DIRECTION('',(0.,0.,1.));
#6405=DIRECTION('',(2.22044604925031E-16,-1.,0.));
#6406=DIRECTION('',(0.,-1.,2.22044604925031E-16));
#6407=DIRECTION('',(1.,0.,0.));
#6408=DIRECTION('',(0.,-1.,2.22044604925031E-16));
#6409=DIRECTION('',(1.,0.,0.));
#6410=DIRECTION('',(0.,0.,1.));
#6411=DIRECTION('',(-1.,1.22464679914735E-16,0.));
#6412=DIRECTION('',(0.,-1.,2.22044604925031E-16));
#6413=DIRECTION('',(1.,0.,0.));
#6414=DIRECTION('',(0.,-1.,2.22044604925031E-16));
#6415=DIRECTION('',(1.,0.,0.));
#6416=DIRECTION('',(0.,-1.,2.22044604925031E-16));
#6417=DIRECTION('',(1.,0.,0.));
#6418=DIRECTION('',(0.,-1.,2.22044604925031E-16));
#6419=DIRECTION('',(1.,0.,0.));
#6420=DIRECTION('axis',(0.,0.,1.));
#6421=DIRECTION('refdir',(1.,0.,0.));
#6422=DIRECTION('center_axis',(0.,1.,0.));
#6423=DIRECTION('ref_axis',(1.,0.,0.));
#6424=DIRECTION('center_axis',(0.,-1.,0.));
#6425=DIRECTION('ref_axis',(1.,0.,0.));
#6426=DIRECTION('',(0.,-1.,0.));
#6427=DIRECTION('center_axis',(0.,-1.,0.));
#6428=DIRECTION('ref_axis',(1.,0.,0.));
#6429=DIRECTION('center_axis',(0.,1.,0.));
#6430=DIRECTION('ref_axis',(1.,0.,0.));
#6431=DIRECTION('center_axis',(0.,1.,0.));
#6432=DIRECTION('ref_axis',(1.,0.,0.));
#6433=DIRECTION('',(0.,-1.,0.));
#6434=DIRECTION('center_axis',(0.,1.,0.));
#6435=DIRECTION('ref_axis',(1.,0.,0.));
#6436=DIRECTION('center_axis',(0.,1.,0.));
#6437=DIRECTION('ref_axis',(1.,0.,0.));
#6438=DIRECTION('center_axis',(0.,1.,0.));
#6439=DIRECTION('ref_axis',(1.,0.,0.));
#6440=DIRECTION('axis',(0.,0.,1.));
#6441=DIRECTION('refdir',(1.,0.,0.));
#6442=DIRECTION('center_axis',(0.,1.,0.));
#6443=DIRECTION('ref_axis',(0.,0.,1.));
#6444=DIRECTION('center_axis',(0.,-1.,0.));
#6445=DIRECTION('ref_axis',(1.,0.,0.));
#6446=DIRECTION('center_axis',(0.,-1.,0.));
#6447=DIRECTION('ref_axis',(1.,0.,0.));
#6448=DIRECTION('center_axis',(0.,-1.,0.));
#6449=DIRECTION('ref_axis',(1.,0.,0.));
#6450=DIRECTION('',(0.707106781186548,0.707106781186547,8.65956056235494E-17));
#6451=DIRECTION('center_axis',(0.,-1.,0.));
#6452=DIRECTION('ref_axis',(1.,0.,0.));
#6453=DIRECTION('center_axis',(0.,-1.,0.));
#6454=DIRECTION('ref_axis',(1.,0.,0.));
#6455=DIRECTION('',(0.,1.,0.));
#6456=DIRECTION('center_axis',(0.,1.,0.));
#6457=DIRECTION('ref_axis',(1.,0.,0.));
#6458=DIRECTION('center_axis',(0.,-1.,0.));
#6459=DIRECTION('ref_axis',(1.,0.,0.));
#6460=DIRECTION('',(-0.707106781186547,0.707106781186548,-8.65956056235493E-17));
#6461=DIRECTION('center_axis',(0.,-1.,0.));
#6462=DIRECTION('ref_axis',(0.,0.,-1.));
#6463=DIRECTION('center_axis',(0.,-1.,0.));
#6464=DIRECTION('ref_axis',(1.,0.,0.));
#6465=DIRECTION('center_axis',(0.,1.,0.));
#6466=DIRECTION('ref_axis',(1.,0.,0.));
#6467=DIRECTION('center_axis',(0.,1.,0.));
#6468=DIRECTION('ref_axis',(1.,0.,0.));
#6469=DIRECTION('',(-0.447213595499958,0.894427190999916,-5.47678698264203E-17));
#6470=DIRECTION('center_axis',(0.,-1.,0.));
#6471=DIRECTION('ref_axis',(1.,0.,0.));
#6472=DIRECTION('center_axis',(0.,1.,0.));
#6473=DIRECTION('ref_axis',(1.,0.,0.));
#6474=DIRECTION('',(0.,1.,0.));
#6475=DIRECTION('center_axis',(0.,1.,0.));
#6476=DIRECTION('ref_axis',(1.,0.,0.));
#6477=DIRECTION('center_axis',(0.,-1.,0.));
#6478=DIRECTION('ref_axis',(1.,0.,0.));
#6479=DIRECTION('',(-0.707106781186547,0.707106781186548,-8.65956056235493E-17));
#6480=DIRECTION('center_axis',(0.,-1.,0.));
#6481=DIRECTION('ref_axis',(0.,0.,-1.));
#6482=DIRECTION('center_axis',(0.866025403784439,0.,-0.5));
#6483=DIRECTION('ref_axis',(0.5,0.,0.866025403784439));
#6484=DIRECTION('',(-0.5,0.,-0.866025403784439));
#6485=DIRECTION('',(0.,-1.,0.));
#6486=DIRECTION('',(0.5,0.,0.866025403784439));
#6487=DIRECTION('',(0.,-1.,0.));
#6488=DIRECTION('center_axis',(1.92296268638356E-16,0.,-1.));
#6489=DIRECTION('ref_axis',(1.,0.,1.92296268638356E-16));
#6490=DIRECTION('',(-1.,0.,-1.92296268638356E-16));
#6491=DIRECTION('',(0.,-1.,0.));
#6492=DIRECTION('',(1.,0.,1.92296268638356E-16));
#6493=DIRECTION('center_axis',(-0.866025403784439,0.,-0.5));
#6494=DIRECTION('ref_axis',(0.5,0.,-0.866025403784439));
#6495=DIRECTION('',(-0.5,0.,0.866025403784438));
#6496=DIRECTION('',(0.,-1.,0.));
#6497=DIRECTION('',(0.5,0.,-0.866025403784438));
#6498=DIRECTION('center_axis',(-0.866025403784439,0.,0.5));
#6499=DIRECTION('ref_axis',(-0.5,0.,-0.866025403784439));
#6500=DIRECTION('',(0.5,0.,0.866025403784439));
#6501=DIRECTION('',(0.,-1.,0.));
#6502=DIRECTION('',(-0.5,0.,-0.866025403784439));
#6503=DIRECTION('center_axis',(-1.92296268638356E-16,0.,1.));
#6504=DIRECTION('ref_axis',(-1.,0.,-1.92296268638356E-16));
#6505=DIRECTION('',(1.,0.,1.92296268638356E-16));
#6506=DIRECTION('',(0.,-1.,0.));
#6507=DIRECTION('',(-1.,0.,-1.92296268638356E-16));
#6508=DIRECTION('center_axis',(0.866025403784439,0.,0.5));
#6509=DIRECTION('ref_axis',(-0.5,0.,0.866025403784439));
#6510=DIRECTION('',(0.5,0.,-0.866025403784439));
#6511=DIRECTION('',(-0.5,0.,0.866025403784439));
#6512=DIRECTION('center_axis',(0.,1.,0.));
#6513=DIRECTION('ref_axis',(1.,0.,0.));
#6514=DIRECTION('center_axis',(0.,-1.,0.));
#6515=DIRECTION('ref_axis',(0.,0.,-1.));
#6516=DIRECTION('',(0.,0.,1.));
#6517=DIRECTION('',(1.,0.,0.));
#6518=DIRECTION('',(0.,0.,1.));
#6519=DIRECTION('',(1.,0.,0.));
#6520=DIRECTION('',(0.,0.,1.));
#6521=DIRECTION('',(1.,0.,0.));
#6522=DIRECTION('',(0.,0.,1.));
#6523=DIRECTION('',(1.,0.,0.));
#6524=DIRECTION('',(0.,0.,1.));
#6525=DIRECTION('',(1.,0.,0.));
#6526=DIRECTION('',(0.,0.,1.));
#6527=DIRECTION('',(1.,0.,0.));
#6528=DIRECTION('',(0.,0.,1.));
#6529=DIRECTION('',(1.,0.,0.));
#6530=DIRECTION('',(0.,0.,1.));
#6531=DIRECTION('',(2.22044604925031E-16,-1.,0.));
#6532=DIRECTION('',(0.,0.,1.));
#6533=DIRECTION('',(2.22044604925031E-16,-1.,0.));
#6534=DIRECTION('',(0.,0.,1.));
#6535=DIRECTION('',(2.22044604925031E-16,-1.,0.));
#6536=DIRECTION('',(0.,0.,1.));
#6537=DIRECTION('',(2.22044604925031E-16,-1.,0.));
#6538=DIRECTION('',(0.,0.,1.));
#6539=DIRECTION('',(2.22044604925031E-16,1.,0.));
#6540=DIRECTION('',(0.,0.,1.));
#6541=DIRECTION('',(2.22044604925031E-16,1.,0.));
#6542=DIRECTION('',(0.,0.,1.));
#6543=DIRECTION('',(2.22044604925031E-16,1.,0.));
#6544=DIRECTION('',(0.,0.,1.));
#6545=DIRECTION('',(2.22044604925031E-16,1.,0.));
#6546=DIRECTION('',(0.,0.,1.));
#6547=DIRECTION('',(2.22044604925031E-16,-1.,0.));
#6548=DIRECTION('',(0.,0.,1.));
#6549=DIRECTION('',(2.22044604925031E-16,-1.,0.));
#6550=DIRECTION('',(0.,0.,1.));
#6551=DIRECTION('',(2.22044604925031E-16,-1.,0.));
#6552=DIRECTION('',(0.,0.,1.));
#6553=DIRECTION('',(2.22044604925031E-16,-1.,0.));
#6554=DIRECTION('',(0.,-1.,2.22044604925031E-16));
#6555=DIRECTION('',(1.,0.,0.));
#6556=DIRECTION('',(0.,-1.,2.22044604925031E-16));
#6557=DIRECTION('',(1.,0.,0.));
#6558=DIRECTION('',(0.,-1.,2.22044604925031E-16));
#6559=DIRECTION('',(1.,0.,0.));
#6560=DIRECTION('',(0.,-1.,2.22044604925031E-16));
#6561=DIRECTION('',(1.,0.,0.));
#6562=DIRECTION('',(0.,-1.,2.22044604925031E-16));
#6563=DIRECTION('',(1.,0.,0.));
#6564=DIRECTION('',(0.,-1.,2.22044604925031E-16));
#6565=DIRECTION('',(1.,0.,0.));
#6566=DIRECTION('',(0.,0.,1.));
#6567=DIRECTION('',(1.,0.,0.));
#6568=DIRECTION('',(0.,0.,1.));
#6569=DIRECTION('',(1.,0.,0.));
#6570=CARTESIAN_POINT('',(0.,0.,0.));
#6571=CARTESIAN_POINT('',(0.,0.,0.));
#6572=CARTESIAN_POINT('',(0.,0.,0.));
#6573=CARTESIAN_POINT('Origin',(26.5,-5.5,-0.1));
#6574=CARTESIAN_POINT('',(26.29,-5.5,0.));
#6575=CARTESIAN_POINT('Origin',(26.5,-5.5,0.));
#6576=CARTESIAN_POINT('',(26.29,-5.5,1.));
#6577=CARTESIAN_POINT('',(26.29,-5.5,-0.1));
#6578=CARTESIAN_POINT('Origin',(26.5,-5.5,1.));
#6579=CARTESIAN_POINT('Origin',(3.5,5.5,-0.1));
#6580=CARTESIAN_POINT('',(3.29,5.5,0.));
#6581=CARTESIAN_POINT('Origin',(3.5,5.5,0.));
#6582=CARTESIAN_POINT('',(3.29,5.5,1.));
#6583=CARTESIAN_POINT('',(3.29,5.5,-0.1));
#6584=CARTESIAN_POINT('Origin',(3.5,5.5,1.));
#6585=CARTESIAN_POINT('Origin',(3.5,-5.5,-0.1));
#6586=CARTESIAN_POINT('',(3.29,-5.5,0.));
#6587=CARTESIAN_POINT('Origin',(3.5,-5.5,0.));
#6588=CARTESIAN_POINT('',(3.29,-5.5,1.));
#6589=CARTESIAN_POINT('',(3.29,-5.5,-0.1));
#6590=CARTESIAN_POINT('Origin',(3.5,-5.5,1.));
#6591=CARTESIAN_POINT('Origin',(26.5,5.5,-0.1));
#6592=CARTESIAN_POINT('',(26.29,5.5,0.));
#6593=CARTESIAN_POINT('Origin',(26.5,5.5,0.));
#6594=CARTESIAN_POINT('',(26.29,5.5,1.));
#6595=CARTESIAN_POINT('',(26.29,5.5,-0.1));
#6596=CARTESIAN_POINT('Origin',(26.5,5.5,1.));
#6597=CARTESIAN_POINT('Origin',(29.,2.4,-0.1));
#6598=CARTESIAN_POINT('',(28.79,2.4,0.));
#6599=CARTESIAN_POINT('Origin',(29.,2.4,0.));
#6600=CARTESIAN_POINT('',(28.79,2.4,1.));
#6601=CARTESIAN_POINT('',(28.79,2.4,-0.1));
#6602=CARTESIAN_POINT('Origin',(29.,2.4,1.));
#6603=CARTESIAN_POINT('Origin',(29.,-5.6,-0.1));
#6604=CARTESIAN_POINT('',(28.79,-5.6,0.));
#6605=CARTESIAN_POINT('Origin',(29.,-5.6,0.));
#6606=CARTESIAN_POINT('',(28.79,-5.6,1.));
#6607=CARTESIAN_POINT('',(28.79,-5.6,-0.1));
#6608=CARTESIAN_POINT('Origin',(29.,-5.6,1.));
#6609=CARTESIAN_POINT('Origin',(1.,5.6,-0.1));
#6610=CARTESIAN_POINT('',(0.79,5.6,0.));
#6611=CARTESIAN_POINT('Origin',(1.,5.6,0.));
#6612=CARTESIAN_POINT('',(0.79,5.6,1.));
#6613=CARTESIAN_POINT('',(0.79,5.6,-0.1));
#6614=CARTESIAN_POINT('Origin',(1.,5.6,1.));
#6615=CARTESIAN_POINT('Origin',(1.,-2.4,-0.1));
#6616=CARTESIAN_POINT('',(0.79,-2.4,0.));
#6617=CARTESIAN_POINT('Origin',(1.,-2.4,0.));
#6618=CARTESIAN_POINT('',(0.79,-2.4,1.));
#6619=CARTESIAN_POINT('',(0.79,-2.4,-0.1));
#6620=CARTESIAN_POINT('Origin',(1.,-2.4,1.));
#6621=CARTESIAN_POINT('Origin',(1.,2.4,-0.1));
#6622=CARTESIAN_POINT('',(0.79,2.4,0.));
#6623=CARTESIAN_POINT('Origin',(1.,2.4,0.));
#6624=CARTESIAN_POINT('',(0.79,2.4,1.));
#6625=CARTESIAN_POINT('',(0.79,2.4,-0.1));
#6626=CARTESIAN_POINT('Origin',(1.,2.4,1.));
#6627=CARTESIAN_POINT('Origin',(1.,-5.6,-0.1));
#6628=CARTESIAN_POINT('',(0.79,-5.6,0.));
#6629=CARTESIAN_POINT('Origin',(1.,-5.6,0.));
#6630=CARTESIAN_POINT('',(0.79,-5.6,1.));
#6631=CARTESIAN_POINT('',(0.79,-5.6,-0.1));
#6632=CARTESIAN_POINT('Origin',(1.,-5.6,1.));
#6633=CARTESIAN_POINT('Origin',(29.,-2.4,-0.1));
#6634=CARTESIAN_POINT('',(28.79,-2.4,0.));
#6635=CARTESIAN_POINT('Origin',(29.,-2.4,0.));
#6636=CARTESIAN_POINT('',(28.79,-2.4,1.));
#6637=CARTESIAN_POINT('',(28.79,-2.4,-0.1));
#6638=CARTESIAN_POINT('Origin',(29.,-2.4,1.));
#6639=CARTESIAN_POINT('Origin',(29.,5.6,-0.1));
#6640=CARTESIAN_POINT('',(28.79,5.6,0.));
#6641=CARTESIAN_POINT('Origin',(29.,5.6,0.));
#6642=CARTESIAN_POINT('',(28.79,5.6,1.));
#6643=CARTESIAN_POINT('',(28.79,5.6,-0.1));
#6644=CARTESIAN_POINT('Origin',(29.,5.6,1.));
#6645=CARTESIAN_POINT('Origin',(31.,7.5,0.));
#6646=CARTESIAN_POINT('',(31.,7.5,0.));
#6647=CARTESIAN_POINT('',(-1.,7.5,0.));
#6648=CARTESIAN_POINT('',(31.,7.5,0.));
#6649=CARTESIAN_POINT('',(-1.,7.5,1.));
#6650=CARTESIAN_POINT('',(-1.,7.5,0.));
#6651=CARTESIAN_POINT('',(31.,7.5,1.));
#6652=CARTESIAN_POINT('',(31.,7.5,1.));
#6653=CARTESIAN_POINT('',(31.,7.5,0.));
#6654=CARTESIAN_POINT('Origin',(31.,-7.5,0.));
#6655=CARTESIAN_POINT('',(31.,-7.5,0.));
#6656=CARTESIAN_POINT('',(31.,-7.5,0.));
#6657=CARTESIAN_POINT('',(31.,-7.5,1.));
#6658=CARTESIAN_POINT('',(31.,-7.5,1.));
#6659=CARTESIAN_POINT('',(31.,-7.5,0.));
#6660=CARTESIAN_POINT('Origin',(-1.,-7.5,0.));
#6661=CARTESIAN_POINT('',(-1.,-7.5,0.));
#6662=CARTESIAN_POINT('',(-1.,-7.5,0.));
#6663=CARTESIAN_POINT('',(-1.,-7.5,1.));
#6664=CARTESIAN_POINT('',(-1.,-7.5,1.));
#6665=CARTESIAN_POINT('',(-1.,-7.5,0.));
#6666=CARTESIAN_POINT('Origin',(-1.,7.5,0.));
#6667=CARTESIAN_POINT('',(-1.,7.5,0.));
#6668=CARTESIAN_POINT('',(-1.,7.5,1.));
#6669=CARTESIAN_POINT('Origin',(15.,0.,1.));
#6670=CARTESIAN_POINT('Origin',(15.,0.,0.));
#6671=CARTESIAN_POINT('',(0.,0.,0.));
#6672=CARTESIAN_POINT('Origin',(3.5,-5.5,2.));
#6673=CARTESIAN_POINT('',(3.025,-5.5,2.));
#6674=CARTESIAN_POINT('Origin',(3.5,-5.5,2.));
#6675=CARTESIAN_POINT('',(3.025,-5.5,2.5));
#6676=CARTESIAN_POINT('',(3.025,-5.5,2.));
#6677=CARTESIAN_POINT('Origin',(3.5,-5.5,2.5));
#6678=CARTESIAN_POINT('Origin',(3.5,-5.5,2.));
#6679=CARTESIAN_POINT('',(3.225,-5.5,2.));
#6680=CARTESIAN_POINT('Origin',(3.5,-5.5,2.));
#6681=CARTESIAN_POINT('Origin',(3.5,5.5,2.));
#6682=CARTESIAN_POINT('',(3.025,5.5,2.));
#6683=CARTESIAN_POINT('Origin',(3.5,5.5,2.));
#6684=CARTESIAN_POINT('',(3.025,5.5,2.5));
#6685=CARTESIAN_POINT('',(3.025,5.5,2.));
#6686=CARTESIAN_POINT('Origin',(3.5,5.5,2.5));
#6687=CARTESIAN_POINT('Origin',(3.5,5.5,2.));
#6688=CARTESIAN_POINT('',(3.225,5.5,2.));
#6689=CARTESIAN_POINT('Origin',(3.5,5.5,2.));
#6690=CARTESIAN_POINT('Origin',(3.5,-5.5,0.9));
#6691=CARTESIAN_POINT('',(3.225,-5.5,1.));
#6692=CARTESIAN_POINT('Origin',(3.5,-5.5,1.));
#6693=CARTESIAN_POINT('',(3.225,-5.5,0.9));
#6694=CARTESIAN_POINT('Origin',(3.5,5.5,0.9));
#6695=CARTESIAN_POINT('',(3.225,5.5,1.));
#6696=CARTESIAN_POINT('Origin',(3.5,5.5,1.));
#6697=CARTESIAN_POINT('',(3.225,5.5,0.9));
#6698=CARTESIAN_POINT('Origin',(4.,6.5,1.));
#6699=CARTESIAN_POINT('',(4.,6.5,1.));
#6700=CARTESIAN_POINT('',(3.,6.5,1.));
#6701=CARTESIAN_POINT('',(4.,6.5,1.));
#6702=CARTESIAN_POINT('',(3.,6.5,2.5));
#6703=CARTESIAN_POINT('',(3.,6.5,1.));
#6704=CARTESIAN_POINT('',(4.,6.5,2.5));
#6705=CARTESIAN_POINT('',(4.,6.5,2.5));
#6706=CARTESIAN_POINT('',(4.,6.5,1.));
#6707=CARTESIAN_POINT('Origin',(4.,-6.5,1.));
#6708=CARTESIAN_POINT('',(4.,-6.5,1.));
#6709=CARTESIAN_POINT('',(4.,-6.5,1.));
#6710=CARTESIAN_POINT('',(4.,-6.5,2.5));
#6711=CARTESIAN_POINT('',(4.,-6.5,2.5));
#6712=CARTESIAN_POINT('',(4.,-6.5,1.));
#6713=CARTESIAN_POINT('Origin',(3.,-6.5,1.));
#6714=CARTESIAN_POINT('',(3.,-6.5,1.));
#6715=CARTESIAN_POINT('',(3.,-6.5,1.));
#6716=CARTESIAN_POINT('',(3.,-6.5,2.5));
#6717=CARTESIAN_POINT('',(3.,-6.5,2.5));
#6718=CARTESIAN_POINT('',(3.,-6.5,1.));
#6719=CARTESIAN_POINT('Origin',(3.,6.5,1.));
#6720=CARTESIAN_POINT('',(3.,6.5,1.));
#6721=CARTESIAN_POINT('',(3.,6.5,2.5));
#6722=CARTESIAN_POINT('Origin',(3.5,0.,2.5));
#6723=CARTESIAN_POINT('Origin',(3.5,0.,1.));
#6724=CARTESIAN_POINT('',(0.,0.,0.));
#6725=CARTESIAN_POINT('Origin',(4.2,6.,1.6));
#6726=CARTESIAN_POINT('',(4.2,6.,1.6));
#6727=CARTESIAN_POINT('',(4.,6.,1.6));
#6728=CARTESIAN_POINT('',(4.2,6.,1.6));
#6729=CARTESIAN_POINT('',(4.,6.,2.5));
#6730=CARTESIAN_POINT('',(4.,6.,1.6));
#6731=CARTESIAN_POINT('',(4.2,6.,2.5));
#6732=CARTESIAN_POINT('',(4.2,6.,2.5));
#6733=CARTESIAN_POINT('',(4.2,6.,1.6));
#6734=CARTESIAN_POINT('Origin',(4.2,-6.,1.6));
#6735=CARTESIAN_POINT('',(4.2,-6.,1.6));
#6736=CARTESIAN_POINT('',(4.2,-6.,1.6));
#6737=CARTESIAN_POINT('',(4.2,-6.,2.5));
#6738=CARTESIAN_POINT('',(4.2,-6.,2.5));
#6739=CARTESIAN_POINT('',(4.2,-6.,1.6));
#6740=CARTESIAN_POINT('Origin',(4.,-6.,1.6));
#6741=CARTESIAN_POINT('',(4.,-6.,1.6));
#6742=CARTESIAN_POINT('',(4.,-6.,1.6));
#6743=CARTESIAN_POINT('',(4.,-6.,2.5));
#6744=CARTESIAN_POINT('',(4.,-6.,2.5));
#6745=CARTESIAN_POINT('',(4.,-6.,1.6));
#6746=CARTESIAN_POINT('Origin',(4.,6.,1.6));
#6747=CARTESIAN_POINT('',(4.,6.,1.6));
#6748=CARTESIAN_POINT('',(4.,6.,2.5));
#6749=CARTESIAN_POINT('Origin',(4.1,0.,2.5));
#6750=CARTESIAN_POINT('Origin',(4.1,0.,1.6));
#6751=CARTESIAN_POINT('',(0.,0.,0.));
#6752=CARTESIAN_POINT('Origin',(26.5,-5.5,2.));
#6753=CARTESIAN_POINT('',(26.025,-5.5,2.));
#6754=CARTESIAN_POINT('Origin',(26.5,-5.5,2.));
#6755=CARTESIAN_POINT('',(26.025,-5.5,2.5));
#6756=CARTESIAN_POINT('',(26.025,-5.5,2.));
#6757=CARTESIAN_POINT('Origin',(26.5,-5.5,2.5));
#6758=CARTESIAN_POINT('Origin',(26.5,-5.5,2.));
#6759=CARTESIAN_POINT('',(26.225,-5.5,2.));
#6760=CARTESIAN_POINT('Origin',(26.5,-5.5,2.));
#6761=CARTESIAN_POINT('Origin',(26.5,5.5,2.));
#6762=CARTESIAN_POINT('',(26.025,5.5,2.));
#6763=CARTESIAN_POINT('Origin',(26.5,5.5,2.));
#6764=CARTESIAN_POINT('',(26.025,5.5,2.5));
#6765=CARTESIAN_POINT('',(26.025,5.5,2.));
#6766=CARTESIAN_POINT('Origin',(26.5,5.5,2.5));
#6767=CARTESIAN_POINT('Origin',(26.5,5.5,2.));
#6768=CARTESIAN_POINT('',(26.225,5.5,2.));
#6769=CARTESIAN_POINT('Origin',(26.5,5.5,2.));
#6770=CARTESIAN_POINT('Origin',(26.5,-5.5,0.9));
#6771=CARTESIAN_POINT('',(26.225,-5.5,1.));
#6772=CARTESIAN_POINT('Origin',(26.5,-5.5,1.));
#6773=CARTESIAN_POINT('',(26.225,-5.5,0.9));
#6774=CARTESIAN_POINT('Origin',(26.5,5.5,0.9));
#6775=CARTESIAN_POINT('',(26.225,5.5,1.));
#6776=CARTESIAN_POINT('Origin',(26.5,5.5,1.));
#6777=CARTESIAN_POINT('',(26.225,5.5,0.9));
#6778=CARTESIAN_POINT('Origin',(27.,6.5,1.));
#6779=CARTESIAN_POINT('',(27.,6.5,1.));
#6780=CARTESIAN_POINT('',(26.,6.5,1.));
#6781=CARTESIAN_POINT('',(27.,6.5,1.));
#6782=CARTESIAN_POINT('',(26.,6.5,2.5));
#6783=CARTESIAN_POINT('',(26.,6.5,1.));
#6784=CARTESIAN_POINT('',(27.,6.5,2.5));
#6785=CARTESIAN_POINT('',(27.,6.5,2.5));
#6786=CARTESIAN_POINT('',(27.,6.5,1.));
#6787=CARTESIAN_POINT('Origin',(27.,-6.5,1.));
#6788=CARTESIAN_POINT('',(27.,-6.5,1.));
#6789=CARTESIAN_POINT('',(27.,-6.5,1.));
#6790=CARTESIAN_POINT('',(27.,-6.5,2.5));
#6791=CARTESIAN_POINT('',(27.,-6.5,2.5));
#6792=CARTESIAN_POINT('',(27.,-6.5,1.));
#6793=CARTESIAN_POINT('Origin',(26.,-6.5,1.));
#6794=CARTESIAN_POINT('',(26.,-6.5,1.));
#6795=CARTESIAN_POINT('',(26.,-6.5,1.));
#6796=CARTESIAN_POINT('',(26.,-6.5,2.5));
#6797=CARTESIAN_POINT('',(26.,-6.5,2.5));
#6798=CARTESIAN_POINT('',(26.,-6.5,1.));
#6799=CARTESIAN_POINT('Origin',(26.,6.5,1.));
#6800=CARTESIAN_POINT('',(26.,6.5,1.));
#6801=CARTESIAN_POINT('',(26.,6.5,2.5));
#6802=CARTESIAN_POINT('Origin',(26.5,0.,2.5));
#6803=CARTESIAN_POINT('Origin',(26.5,0.,1.));
#6804=CARTESIAN_POINT('',(0.,0.,0.));
#6805=CARTESIAN_POINT('Origin',(26.,6.,1.6));
#6806=CARTESIAN_POINT('',(26.,6.,1.6));
#6807=CARTESIAN_POINT('',(25.8,6.,1.6));
#6808=CARTESIAN_POINT('',(26.,6.,1.6));
#6809=CARTESIAN_POINT('',(25.8,6.,2.5));
#6810=CARTESIAN_POINT('',(25.8,6.,1.6));
#6811=CARTESIAN_POINT('',(26.,6.,2.5));
#6812=CARTESIAN_POINT('',(26.,6.,2.5));
#6813=CARTESIAN_POINT('',(26.,6.,1.6));
#6814=CARTESIAN_POINT('Origin',(26.,-6.,1.6));
#6815=CARTESIAN_POINT('',(26.,-6.,1.6));
#6816=CARTESIAN_POINT('',(26.,-6.,1.6));
#6817=CARTESIAN_POINT('',(26.,-6.,2.5));
#6818=CARTESIAN_POINT('',(26.,-6.,2.5));
#6819=CARTESIAN_POINT('',(26.,-6.,1.6));
#6820=CARTESIAN_POINT('Origin',(25.8,-6.,1.6));
#6821=CARTESIAN_POINT('',(25.8,-6.,1.6));
#6822=CARTESIAN_POINT('',(25.8,-6.,1.6));
#6823=CARTESIAN_POINT('',(25.8,-6.,2.5));
#6824=CARTESIAN_POINT('',(25.8,-6.,2.5));
#6825=CARTESIAN_POINT('',(25.8,-6.,1.6));
#6826=CARTESIAN_POINT('Origin',(25.8,6.,1.6));
#6827=CARTESIAN_POINT('',(25.8,6.,1.6));
#6828=CARTESIAN_POINT('',(25.8,6.,2.5));
#6829=CARTESIAN_POINT('Origin',(25.9,0.,2.5));
#6830=CARTESIAN_POINT('Origin',(25.9,0.,1.6));
#6831=CARTESIAN_POINT('',(0.,0.,0.));
#6832=CARTESIAN_POINT('Origin',(0.05,0.,0.));
#6833=CARTESIAN_POINT('',(0.1,7.34788079488412E-17,0.6));
#6834=CARTESIAN_POINT('Origin',(0.1,0.,0.));
#6835=CARTESIAN_POINT('',(0.,-6.12323399573677E-17,0.5));
#6836=CARTESIAN_POINT('',(0.05,-6.73555739531044E-17,0.55));
#6837=CARTESIAN_POINT('Origin',(0.,0.,0.));
#6838=CARTESIAN_POINT('Origin',(0.,0.,0.));
#6839=CARTESIAN_POINT('',(29.9,-7.34788079488412E-17,0.6));
#6840=CARTESIAN_POINT('Origin',(29.9,0.,0.));
#6841=CARTESIAN_POINT('',(0.,-7.34788079488412E-17,0.6));
#6842=CARTESIAN_POINT('Origin',(0.,0.,0.));
#6843=CARTESIAN_POINT('Origin',(29.95,0.,0.));
#6844=CARTESIAN_POINT('',(30.,6.12323399573677E-17,0.5));
#6845=CARTESIAN_POINT('Origin',(30.,0.,0.));
#6846=CARTESIAN_POINT('',(29.95,-6.73555739531044E-17,0.55));
#6847=CARTESIAN_POINT('Origin',(30.,0.,0.));
#6848=CARTESIAN_POINT('',(0.,0.,0.));
#6849=CARTESIAN_POINT('Origin',(-1.6,0.,1.3));
#6850=CARTESIAN_POINT('',(-1.2,0.340036762718386,1.3));
#6851=CARTESIAN_POINT('',(-1.2,-0.340036762718386,1.3));
#6852=CARTESIAN_POINT('',(-1.2,0.,1.3));
#6853=CARTESIAN_POINT('Origin',(-1.6,0.,1.3));
#6854=CARTESIAN_POINT('Origin',(-1.6,0.,0.6));
#6855=CARTESIAN_POINT('',(-1.2,0.340036762718386,0.6));
#6856=CARTESIAN_POINT('',(-1.2,0.340036762718386,0.6));
#6857=CARTESIAN_POINT('',(-1.2,-0.340036762718386,0.6));
#6858=CARTESIAN_POINT('Origin',(-1.6,0.,0.6));
#6859=CARTESIAN_POINT('',(-1.2,-0.340036762718386,0.6));
#6860=CARTESIAN_POINT('Origin',(1.6,0.,0.6));
#6861=CARTESIAN_POINT('',(1.2,0.340036762718386,1.3));
#6862=CARTESIAN_POINT('',(1.2,0.340036762718386,0.6));
#6863=CARTESIAN_POINT('',(1.2,0.340036762718386,0.6));
#6864=CARTESIAN_POINT('',(1.2,-0.340036762718386,1.3));
#6865=CARTESIAN_POINT('Origin',(1.6,0.,1.3));
#6866=CARTESIAN_POINT('',(1.2,-0.340036762718386,0.6));
#6867=CARTESIAN_POINT('',(1.2,-0.340036762718386,0.6));
#6868=CARTESIAN_POINT('Origin',(1.6,0.,0.6));
#6869=CARTESIAN_POINT('Origin',(1.6,0.,1.3));
#6870=CARTESIAN_POINT('',(1.2,0.,1.3));
#6871=CARTESIAN_POINT('Origin',(-2.1,0.,0.6));
#6872=CARTESIAN_POINT('',(-1.2,0.7,0.6));
#6873=CARTESIAN_POINT('',(-1.2,0.,0.6));
#6874=CARTESIAN_POINT('',(-2.1,0.7,0.6));
#6875=CARTESIAN_POINT('',(-1.2,0.7,0.6));
#6876=CARTESIAN_POINT('',(-2.1,-0.7,0.6));
#6877=CARTESIAN_POINT('',(-2.1,0.,0.6));
#6878=CARTESIAN_POINT('',(-1.2,-0.7,0.6));
#6879=CARTESIAN_POINT('',(-1.2,-0.7,0.6));
#6880=CARTESIAN_POINT('',(-1.2,0.,0.6));
#6881=CARTESIAN_POINT('',(-1.875,3.36777869765522E-17,0.6));
#6882=CARTESIAN_POINT('Origin',(-1.6,0.,0.6));
#6883=CARTESIAN_POINT('Origin',(-1.2,0.,0.6));
#6884=CARTESIAN_POINT('',(-1.2,-0.7,3.75));
#6885=CARTESIAN_POINT('',(-1.2,-0.7,3.75));
#6886=CARTESIAN_POINT('',(-1.2,0.7,3.75));
#6887=CARTESIAN_POINT('',(-1.2,0.,3.75));
#6888=CARTESIAN_POINT('',(-1.2,0.7,3.75));
#6889=CARTESIAN_POINT('',(-1.2,-2.02066721859313E-17,3.515));
#6890=CARTESIAN_POINT('Origin',(-1.2,0.,3.35));
#6891=CARTESIAN_POINT('Origin',(1.2,0.,0.6));
#6892=CARTESIAN_POINT('',(2.1,-0.7,0.6));
#6893=CARTESIAN_POINT('',(2.1,0.7,0.6));
#6894=CARTESIAN_POINT('',(2.1,0.,0.6));
#6895=CARTESIAN_POINT('',(1.2,0.7,0.6));
#6896=CARTESIAN_POINT('',(2.1,0.7,0.6));
#6897=CARTESIAN_POINT('',(1.2,0.,0.6));
#6898=CARTESIAN_POINT('',(1.2,-0.7,0.6));
#6899=CARTESIAN_POINT('',(1.2,0.,0.6));
#6900=CARTESIAN_POINT('',(2.1,-0.7,0.6));
#6901=CARTESIAN_POINT('',(1.325,3.36777869765522E-17,0.6));
#6902=CARTESIAN_POINT('Origin',(1.6,0.,0.6));
#6903=CARTESIAN_POINT('Origin',(0.1,0.,3.35));
#6904=CARTESIAN_POINT('',(0.1,-2.75545529808155E-17,3.575));
#6905=CARTESIAN_POINT('Origin',(0.1,0.,3.35));
#6906=CARTESIAN_POINT('',(1.2,2.75545529808155E-17,3.575));
#6907=CARTESIAN_POINT('',(0.1,-2.75545529808155E-17,3.575));
#6908=CARTESIAN_POINT('Origin',(1.2,0.,3.35));
#6909=CARTESIAN_POINT('Origin',(0.,0.,3.35));
#6910=CARTESIAN_POINT('',(-0.1,2.02066721859313E-17,3.515));
#6911=CARTESIAN_POINT('',(0.,-2.02066721859313E-17,3.515));
#6912=CARTESIAN_POINT('Origin',(-0.1,0.,3.35));
#6913=CARTESIAN_POINT('Origin',(-1.6,0.,-0.05));
#6914=CARTESIAN_POINT('',(-1.875,-3.36777869765522E-17,0.));
#6915=CARTESIAN_POINT('Origin',(-1.6,0.,0.));
#6916=CARTESIAN_POINT('',(-1.875,-3.36777869765522E-17,-0.05));
#6917=CARTESIAN_POINT('Origin',(1.6,0.,-0.05));
#6918=CARTESIAN_POINT('',(1.325,-3.36777869765522E-17,0.));
#6919=CARTESIAN_POINT('Origin',(1.6,0.,0.));
#6920=CARTESIAN_POINT('',(1.325,-3.36777869765522E-17,-0.05));
#6921=CARTESIAN_POINT('Origin',(0.,0.,2.3));
#6922=CARTESIAN_POINT('',(-0.6,-0.7,2.3));
#6923=CARTESIAN_POINT('Origin',(0.,-0.7,2.3));
#6924=CARTESIAN_POINT('',(-0.6,0.7,2.3));
#6925=CARTESIAN_POINT('',(-0.6,0.,2.3));
#6926=CARTESIAN_POINT('Origin',(0.,0.7,2.3));
#6927=CARTESIAN_POINT('Origin',(0.,-0.7,1.875));
#6928=CARTESIAN_POINT('',(-2.1,-0.7,0.));
#6929=CARTESIAN_POINT('',(-2.1,-0.7,0.6));
#6930=CARTESIAN_POINT('',(2.1,-0.7,0.));
#6931=CARTESIAN_POINT('',(-2.1,-0.7,0.));
#6932=CARTESIAN_POINT('',(2.1,-0.7,0.));
#6933=CARTESIAN_POINT('',(1.2,-0.7,3.75));
#6934=CARTESIAN_POINT('',(1.2,-0.7,0.6));
#6935=CARTESIAN_POINT('',(0.1,-0.7,3.75));
#6936=CARTESIAN_POINT('',(1.2,-0.7,3.75));
#6937=CARTESIAN_POINT('',(0.1,-0.7,2.95));
#6938=CARTESIAN_POINT('',(0.1,-0.7,3.75));
#6939=CARTESIAN_POINT('',(-0.1,-0.7,2.95));
#6940=CARTESIAN_POINT('',(0.1,-0.7,2.95));
#6941=CARTESIAN_POINT('',(-0.1,-0.7,3.75));
#6942=CARTESIAN_POINT('',(-0.1,-0.7,2.95));
#6943=CARTESIAN_POINT('',(-0.1,-0.7,3.75));
#6944=CARTESIAN_POINT('Origin',(-2.1,0.,0.));
#6945=CARTESIAN_POINT('',(-2.1,0.7,0.));
#6946=CARTESIAN_POINT('',(-2.1,0.7,0.6));
#6947=CARTESIAN_POINT('',(-2.1,0.,0.));
#6948=CARTESIAN_POINT('Origin',(2.1,0.,0.));
#6949=CARTESIAN_POINT('',(2.1,0.7,0.));
#6950=CARTESIAN_POINT('',(-2.1,0.7,0.));
#6951=CARTESIAN_POINT('',(2.1,0.,0.));
#6952=CARTESIAN_POINT('Origin',(2.1,0.,0.6));
#6953=CARTESIAN_POINT('',(2.1,0.7,0.));
#6954=CARTESIAN_POINT('Origin',(1.2,0.,3.75));
#6955=CARTESIAN_POINT('',(1.2,0.7,3.75));
#6956=CARTESIAN_POINT('',(1.2,0.7,0.6));
#6957=CARTESIAN_POINT('',(1.2,0.,3.75));
#6958=CARTESIAN_POINT('Origin',(0.1,0.,3.75));
#6959=CARTESIAN_POINT('',(0.1,0.7,3.75));
#6960=CARTESIAN_POINT('',(1.2,0.7,3.75));
#6961=CARTESIAN_POINT('',(0.1,0.,3.75));
#6962=CARTESIAN_POINT('Origin',(0.1,0.,2.95));
#6963=CARTESIAN_POINT('',(0.1,0.7,2.95));
#6964=CARTESIAN_POINT('',(0.1,0.7,3.75));
#6965=CARTESIAN_POINT('',(0.1,0.,2.95));
#6966=CARTESIAN_POINT('Origin',(-0.1,0.,2.95));
#6967=CARTESIAN_POINT('',(-0.1,0.7,2.95));
#6968=CARTESIAN_POINT('',(0.1,0.7,2.95));
#6969=CARTESIAN_POINT('',(-0.1,0.,2.95));
#6970=CARTESIAN_POINT('Origin',(-0.1,0.,3.75));
#6971=CARTESIAN_POINT('',(-0.1,0.7,3.75));
#6972=CARTESIAN_POINT('',(-0.1,0.7,2.95));
#6973=CARTESIAN_POINT('',(-0.1,0.,3.75));
#6974=CARTESIAN_POINT('Origin',(-1.2,0.,3.75));
#6975=CARTESIAN_POINT('',(-0.1,0.7,3.75));
#6976=CARTESIAN_POINT('Origin',(0.,0.7,1.875));
#6977=CARTESIAN_POINT('',(0.,0.,0.));
#6978=CARTESIAN_POINT('Origin',(0.115470053837925,-0.5,-0.2));
#6979=CARTESIAN_POINT('',(0.23094010767585,-0.5,0.));
#6980=CARTESIAN_POINT('',(0.115470053837925,-0.5,-0.2));
#6981=CARTESIAN_POINT('',(0.23094010767585,-0.5,0.));
#6982=CARTESIAN_POINT('',(0.115470053837925,-0.8,-0.2));
#6983=CARTESIAN_POINT('',(0.115470053837925,-0.5,-0.2));
#6984=CARTESIAN_POINT('',(0.23094010767585,-0.8,0.));
#6985=CARTESIAN_POINT('',(0.23094010767585,-0.8,0.));
#6986=CARTESIAN_POINT('',(0.23094010767585,-0.5,0.));
#6987=CARTESIAN_POINT('Origin',(-0.115470053837925,-0.5,-0.2));
#6988=CARTESIAN_POINT('',(-0.115470053837925,-0.5,-0.2));
#6989=CARTESIAN_POINT('',(0.115470053837925,-0.5,-0.2));
#6990=CARTESIAN_POINT('',(-0.115470053837925,-0.8,-0.2));
#6991=CARTESIAN_POINT('',(-0.115470053837925,-0.5,-0.2));
#6992=CARTESIAN_POINT('',(0.115470053837925,-0.8,-0.2));
#6993=CARTESIAN_POINT('Origin',(-0.23094010767585,-0.5,-2.77555756156289E-17));
#6994=CARTESIAN_POINT('',(-0.23094010767585,-0.5,-2.82820063659975E-17));
#6995=CARTESIAN_POINT('',(-0.115470053837925,-0.5,-0.2));
#6996=CARTESIAN_POINT('',(-0.23094010767585,-0.8,-2.77555756156289E-17));
#6997=CARTESIAN_POINT('',(-0.23094010767585,-0.5,-2.82820063659975E-17));
#6998=CARTESIAN_POINT('',(-0.115470053837925,-0.8,-0.2));
#6999=CARTESIAN_POINT('Origin',(-0.115470053837925,-0.5,0.2));
#7000=CARTESIAN_POINT('',(-0.115470053837925,-0.5,0.2));
#7001=CARTESIAN_POINT('',(-0.23094010767585,-0.5,-2.82820063659975E-17));
#7002=CARTESIAN_POINT('',(-0.115470053837925,-0.8,0.2));
#7003=CARTESIAN_POINT('',(-0.115470053837925,-0.5,0.2));
#7004=CARTESIAN_POINT('',(-0.23094010767585,-0.8,-2.82820063659975E-17));
#7005=CARTESIAN_POINT('Origin',(0.115470053837925,-0.5,0.2));
#7006=CARTESIAN_POINT('',(0.115470053837925,-0.5,0.2));
#7007=CARTESIAN_POINT('',(-0.115470053837925,-0.5,0.2));
#7008=CARTESIAN_POINT('',(0.115470053837925,-0.8,0.2));
#7009=CARTESIAN_POINT('',(0.115470053837925,-0.5,0.2));
#7010=CARTESIAN_POINT('',(-0.115470053837925,-0.8,0.2));
#7011=CARTESIAN_POINT('Origin',(0.23094010767585,-0.5,0.));
#7012=CARTESIAN_POINT('',(0.115470053837925,-0.5,0.2));
#7013=CARTESIAN_POINT('',(0.115470053837925,-0.8,0.2));
#7014=CARTESIAN_POINT('Origin',(0.,-0.5,0.));
#7015=CARTESIAN_POINT('Origin',(0.,-0.8,0.));
#7016=CARTESIAN_POINT('Origin',(0.,-1.4,0.));
#7017=CARTESIAN_POINT('',(-0.24505,-1.4,3.00099698131059E-17));
#7018=CARTESIAN_POINT('Origin',(0.,-1.4,0.));
#7019=CARTESIAN_POINT('Origin',(0.375,0.5,0.));
#7020=CARTESIAN_POINT('',(-0.375,0.5,-4.59242549680257E-17));
#7021=CARTESIAN_POINT('Origin',(0.,0.5,0.));
#7022=CARTESIAN_POINT('Origin',(0.,0.475,0.));
#7023=CARTESIAN_POINT('',(-0.425,0.45,-5.20474889637625E-17));
#7024=CARTESIAN_POINT('Origin',(0.,0.45,0.));
#7025=CARTESIAN_POINT('',(-0.4,0.475,-4.89858719658941E-17));
#7026=CARTESIAN_POINT('Origin',(0.,0.24,0.));
#7027=CARTESIAN_POINT('',(-0.425,0.0299999999999998,-5.20474889637625E-17));
#7028=CARTESIAN_POINT('Origin',(0.,0.0299999999999998,0.));
#7029=CARTESIAN_POINT('',(-0.425,0.24,-5.20474889637625E-17));
#7030=CARTESIAN_POINT('Origin',(0.,0.0150000000000001,0.));
#7031=CARTESIAN_POINT('',(-0.395,4.85722573273506E-17,-4.83735485663204E-17));
#7032=CARTESIAN_POINT('Origin',(0.,0.,0.));
#7033=CARTESIAN_POINT('',(-0.41,0.0150000000000001,-5.02105187650415E-17));
#7034=CARTESIAN_POINT('Origin',(0.27,0.,0.));
#7035=CARTESIAN_POINT('',(-0.27,0.,-3.30654635769785E-17));
#7036=CARTESIAN_POINT('Origin',(0.,0.,0.));
#7037=CARTESIAN_POINT('Origin',(0.,-0.02,0.));
#7038=CARTESIAN_POINT('',(-0.24505,-0.0498999999999999,3.00099698131059E-17));
#7039=CARTESIAN_POINT('Origin',(0.,-0.0498999999999999,0.));
#7040=CARTESIAN_POINT('',(-0.26,-0.02,-3.18408167778312E-17));
#7041=CARTESIAN_POINT('Origin',(0.,-0.995,0.));
#7042=CARTESIAN_POINT('',(-0.24505,-0.995,-3.00099698131059E-17));
#7043=CARTESIAN_POINT('',(0.,0.,0.));
#7044=CARTESIAN_POINT('',(0.,0.,0.));
#7045=CARTESIAN_POINT('Origin',(17.9,5.5,3.));
#7046=CARTESIAN_POINT('',(17.9,5.5,3.165));
#7047=CARTESIAN_POINT('Origin',(17.9,5.5,3.));
#7048=CARTESIAN_POINT('',(19.5,5.5,3.165));
#7049=CARTESIAN_POINT('',(17.9,5.5,3.165));
#7050=CARTESIAN_POINT('Origin',(19.5,5.5,3.));
#7051=CARTESIAN_POINT('Origin',(17.9,5.5,3.));
#7052=CARTESIAN_POINT('Origin',(17.9,-5.5,5.));
#7053=CARTESIAN_POINT('',(17.9,-5.5,5.165));
#7054=CARTESIAN_POINT('Origin',(17.9,-5.5,5.));
#7055=CARTESIAN_POINT('',(19.5,-5.5,5.165));
#7056=CARTESIAN_POINT('',(17.9,-5.5,5.165));
#7057=CARTESIAN_POINT('Origin',(19.5,-5.5,5.));
#7058=CARTESIAN_POINT('Origin',(17.9,-5.5,5.));
#7059=CARTESIAN_POINT('Origin',(17.9,-5.5,3.));
#7060=CARTESIAN_POINT('',(17.9,-5.5,3.165));
#7061=CARTESIAN_POINT('Origin',(17.9,-5.5,3.));
#7062=CARTESIAN_POINT('',(19.5,-5.5,3.165));
#7063=CARTESIAN_POINT('',(17.9,-5.5,3.165));
#7064=CARTESIAN_POINT('Origin',(19.5,-5.5,3.));
#7065=CARTESIAN_POINT('Origin',(17.9,-5.5,3.));
#7066=CARTESIAN_POINT('Origin',(17.9,5.5,5.));
#7067=CARTESIAN_POINT('',(17.9,5.5,5.165));
#7068=CARTESIAN_POINT('Origin',(17.9,5.5,5.));
#7069=CARTESIAN_POINT('',(19.5,5.5,5.165));
#7070=CARTESIAN_POINT('',(17.9,5.5,5.165));
#7071=CARTESIAN_POINT('Origin',(19.5,5.5,5.));
#7072=CARTESIAN_POINT('Origin',(17.9,5.5,5.));
#7073=CARTESIAN_POINT('Origin',(10.5,5.5,3.));
#7074=CARTESIAN_POINT('',(10.5,5.5,3.165));
#7075=CARTESIAN_POINT('Origin',(10.5,5.5,3.));
#7076=CARTESIAN_POINT('',(12.1,5.5,3.165));
#7077=CARTESIAN_POINT('',(10.5,5.5,3.165));
#7078=CARTESIAN_POINT('Origin',(12.1,5.5,3.));
#7079=CARTESIAN_POINT('Origin',(12.1,5.5,3.));
#7080=CARTESIAN_POINT('Origin',(10.5,-5.5,5.));
#7081=CARTESIAN_POINT('',(10.5,-5.5,5.165));
#7082=CARTESIAN_POINT('Origin',(10.5,-5.5,5.));
#7083=CARTESIAN_POINT('',(12.1,-5.5,5.165));
#7084=CARTESIAN_POINT('',(10.5,-5.5,5.165));
#7085=CARTESIAN_POINT('Origin',(12.1,-5.5,5.));
#7086=CARTESIAN_POINT('Origin',(12.1,-5.5,5.));
#7087=CARTESIAN_POINT('Origin',(10.5,-5.5,3.));
#7088=CARTESIAN_POINT('',(10.5,-5.5,3.165));
#7089=CARTESIAN_POINT('Origin',(10.5,-5.5,3.));
#7090=CARTESIAN_POINT('',(12.1,-5.5,3.165));
#7091=CARTESIAN_POINT('',(10.5,-5.5,3.165));
#7092=CARTESIAN_POINT('Origin',(12.1,-5.5,3.));
#7093=CARTESIAN_POINT('Origin',(12.1,-5.5,3.));
#7094=CARTESIAN_POINT('Origin',(10.5,5.5,5.));
#7095=CARTESIAN_POINT('',(10.5,5.5,5.165));
#7096=CARTESIAN_POINT('Origin',(10.5,5.5,5.));
#7097=CARTESIAN_POINT('',(12.1,5.5,5.165));
#7098=CARTESIAN_POINT('',(10.5,5.5,5.165));
#7099=CARTESIAN_POINT('Origin',(12.1,5.5,5.));
#7100=CARTESIAN_POINT('Origin',(12.1,5.5,5.));
#7101=CARTESIAN_POINT('Origin',(18.5,-1.5,4.4));
#7102=CARTESIAN_POINT('',(18.29,-1.5,4.4));
#7103=CARTESIAN_POINT('Origin',(18.5,-1.5,4.4));
#7104=CARTESIAN_POINT('',(18.29,-1.5,5.8));
#7105=CARTESIAN_POINT('',(18.29,-1.5,4.4));
#7106=CARTESIAN_POINT('Origin',(18.5,-1.5,5.8));
#7107=CARTESIAN_POINT('Origin',(18.5,-1.5,4.4));
#7108=CARTESIAN_POINT('Origin',(11.5,1.5,4.4));
#7109=CARTESIAN_POINT('',(11.29,1.5,4.4));
#7110=CARTESIAN_POINT('Origin',(11.5,1.5,4.4));
#7111=CARTESIAN_POINT('',(11.29,1.5,5.8));
#7112=CARTESIAN_POINT('',(11.29,1.5,4.4));
#7113=CARTESIAN_POINT('Origin',(11.5,1.5,5.8));
#7114=CARTESIAN_POINT('Origin',(11.5,1.5,4.4));
#7115=CARTESIAN_POINT('Origin',(11.5,-1.5,4.4));
#7116=CARTESIAN_POINT('',(11.29,-1.5,4.4));
#7117=CARTESIAN_POINT('Origin',(11.5,-1.5,4.4));
#7118=CARTESIAN_POINT('',(11.29,-1.5,5.8));
#7119=CARTESIAN_POINT('',(11.29,-1.5,4.4));
#7120=CARTESIAN_POINT('Origin',(11.5,-1.5,5.8));
#7121=CARTESIAN_POINT('Origin',(11.5,-1.5,4.4));
#7122=CARTESIAN_POINT('Origin',(18.5,1.5,4.4));
#7123=CARTESIAN_POINT('',(18.29,1.5,4.4));
#7124=CARTESIAN_POINT('Origin',(18.5,1.5,4.4));
#7125=CARTESIAN_POINT('',(18.29,1.5,5.8));
#7126=CARTESIAN_POINT('',(18.29,1.5,4.4));
#7127=CARTESIAN_POINT('Origin',(18.5,1.5,5.8));
#7128=CARTESIAN_POINT('Origin',(18.5,1.5,4.4));
#7129=CARTESIAN_POINT('Origin',(10.4,-4.,3.3));
#7130=CARTESIAN_POINT('',(10.5,-4.,4.35));
#7131=CARTESIAN_POINT('Origin',(10.5,-4.,3.3));
#7132=CARTESIAN_POINT('',(19.5,-4.,4.35));
#7133=CARTESIAN_POINT('',(10.4,-4.,4.35));
#7134=CARTESIAN_POINT('Origin',(19.5,-4.,3.3));
#7135=CARTESIAN_POINT('Origin',(10.4,4.,3.3));
#7136=CARTESIAN_POINT('',(10.5,4.,4.35));
#7137=CARTESIAN_POINT('Origin',(10.5,4.,3.3));
#7138=CARTESIAN_POINT('',(19.5,4.,4.35));
#7139=CARTESIAN_POINT('',(10.4,4.,4.35));
#7140=CARTESIAN_POINT('Origin',(19.5,4.,3.3));
#7141=CARTESIAN_POINT('Origin',(19.5,6.,1.6));
#7142=CARTESIAN_POINT('',(19.5,6.,1.6));
#7143=CARTESIAN_POINT('',(10.5,6.,1.6));
#7144=CARTESIAN_POINT('',(19.5,6.,1.6));
#7145=CARTESIAN_POINT('',(10.5,6.,5.8));
#7146=CARTESIAN_POINT('',(10.5,6.,1.6));
#7147=CARTESIAN_POINT('',(19.5,6.,5.8));
#7148=CARTESIAN_POINT('',(19.5,6.,5.8));
#7149=CARTESIAN_POINT('',(19.5,6.,1.6));
#7150=CARTESIAN_POINT('Origin',(19.5,-6.,1.6));
#7151=CARTESIAN_POINT('',(19.5,-6.,1.6));
#7152=CARTESIAN_POINT('',(19.5,-6.,1.6));
#7153=CARTESIAN_POINT('',(19.5,-6.,5.8));
#7154=CARTESIAN_POINT('',(19.5,-6.,5.8));
#7155=CARTESIAN_POINT('',(19.5,-6.,1.6));
#7156=CARTESIAN_POINT('Origin',(10.5,-6.,1.6));
#7157=CARTESIAN_POINT('',(10.5,-6.,1.6));
#7158=CARTESIAN_POINT('',(10.5,-6.,1.6));
#7159=CARTESIAN_POINT('',(10.5,-6.,5.8));
#7160=CARTESIAN_POINT('',(10.5,-6.,5.8));
#7161=CARTESIAN_POINT('',(10.5,-6.,1.6));
#7162=CARTESIAN_POINT('Origin',(10.5,6.,1.6));
#7163=CARTESIAN_POINT('',(10.5,6.,1.6));
#7164=CARTESIAN_POINT('',(10.5,6.,5.8));
#7165=CARTESIAN_POINT('Origin',(15.,0.,5.8));
#7166=CARTESIAN_POINT('Origin',(15.,0.,1.6));
#7167=CARTESIAN_POINT('',(0.,0.,0.));
#7168=CARTESIAN_POINT('Origin',(13.5,-4.,3.3));
#7169=CARTESIAN_POINT('',(16.5,-4.,4.));
#7170=CARTESIAN_POINT('Origin',(16.5,-4.,3.3));
#7171=CARTESIAN_POINT('',(13.5,-4.,4.));
#7172=CARTESIAN_POINT('',(13.5,-4.,4.));
#7173=CARTESIAN_POINT('Origin',(13.5,-4.,3.3));
#7174=CARTESIAN_POINT('Origin',(13.5,-4.,3.3));
#7175=CARTESIAN_POINT('',(16.5,-4.,4.34));
#7176=CARTESIAN_POINT('Origin',(16.5,-4.,3.3));
#7177=CARTESIAN_POINT('',(13.5,-4.,4.34));
#7178=CARTESIAN_POINT('',(13.5,-4.,4.34));
#7179=CARTESIAN_POINT('Origin',(13.5,-4.,3.3));
#7180=CARTESIAN_POINT('Origin',(16.5,-4.,3.3));
#7181=CARTESIAN_POINT('Origin',(13.5,-4.,3.3));
#7182=CARTESIAN_POINT('',(0.,0.,0.));
#7183=CARTESIAN_POINT('Origin',(13.5,4.,3.3));
#7184=CARTESIAN_POINT('',(16.5,4.,4.));
#7185=CARTESIAN_POINT('Origin',(16.5,4.,3.3));
#7186=CARTESIAN_POINT('',(13.5,4.,4.));
#7187=CARTESIAN_POINT('',(13.5,4.,4.));
#7188=CARTESIAN_POINT('Origin',(13.5,4.,3.3));
#7189=CARTESIAN_POINT('Origin',(13.5,4.,3.3));
#7190=CARTESIAN_POINT('',(16.5,4.,4.34));
#7191=CARTESIAN_POINT('Origin',(16.5,4.,3.3));
#7192=CARTESIAN_POINT('',(13.5,4.,4.34));
#7193=CARTESIAN_POINT('',(13.5,4.,4.34));
#7194=CARTESIAN_POINT('Origin',(13.5,4.,3.3));
#7195=CARTESIAN_POINT('Origin',(16.5,4.,3.3));
#7196=CARTESIAN_POINT('Origin',(13.5,4.,3.3));
#7197=CARTESIAN_POINT('',(0.,0.,0.));
#7198=CARTESIAN_POINT('Origin',(9.9,5.5,3.));
#7199=CARTESIAN_POINT('',(10.,5.5,3.225));
#7200=CARTESIAN_POINT('Origin',(10.,5.5,3.));
#7201=CARTESIAN_POINT('',(10.5,5.5,3.225));
#7202=CARTESIAN_POINT('',(9.9,5.5,3.225));
#7203=CARTESIAN_POINT('Origin',(10.5,5.5,3.));
#7204=CARTESIAN_POINT('Origin',(9.9,-5.5,5.));
#7205=CARTESIAN_POINT('',(10.,-5.5,5.225));
#7206=CARTESIAN_POINT('Origin',(10.,-5.5,5.));
#7207=CARTESIAN_POINT('',(10.5,-5.5,5.225));
#7208=CARTESIAN_POINT('',(9.9,-5.5,5.225));
#7209=CARTESIAN_POINT('Origin',(10.5,-5.5,5.));
#7210=CARTESIAN_POINT('Origin',(9.9,-5.5,3.));
#7211=CARTESIAN_POINT('',(10.,-5.5,3.225));
#7212=CARTESIAN_POINT('Origin',(10.,-5.5,3.));
#7213=CARTESIAN_POINT('',(10.5,-5.5,3.225));
#7214=CARTESIAN_POINT('',(9.9,-5.5,3.225));
#7215=CARTESIAN_POINT('Origin',(10.5,-5.5,3.));
#7216=CARTESIAN_POINT('Origin',(9.9,5.5,5.));
#7217=CARTESIAN_POINT('',(10.,5.5,5.225));
#7218=CARTESIAN_POINT('Origin',(10.,5.5,5.));
#7219=CARTESIAN_POINT('',(10.5,5.5,5.225));
#7220=CARTESIAN_POINT('',(9.9,5.5,5.225));
#7221=CARTESIAN_POINT('Origin',(10.5,5.5,5.));
#7222=CARTESIAN_POINT('Origin',(9.9,-4.,3.3));
#7223=CARTESIAN_POINT('',(10.,-4.,4.));
#7224=CARTESIAN_POINT('Origin',(10.,-4.,3.3));
#7225=CARTESIAN_POINT('',(10.5,-4.,4.));
#7226=CARTESIAN_POINT('',(9.9,-4.,4.));
#7227=CARTESIAN_POINT('Origin',(10.5,-4.,3.3));
#7228=CARTESIAN_POINT('Origin',(9.9,4.,3.3));
#7229=CARTESIAN_POINT('',(10.,4.,4.));
#7230=CARTESIAN_POINT('Origin',(10.,4.,3.3));
#7231=CARTESIAN_POINT('',(10.5,4.,4.));
#7232=CARTESIAN_POINT('',(9.9,4.,4.));
#7233=CARTESIAN_POINT('Origin',(10.5,4.,3.3));
#7234=CARTESIAN_POINT('Origin',(10.5,6.,1.6));
#7235=CARTESIAN_POINT('',(10.5,6.,1.6));
#7236=CARTESIAN_POINT('',(10.,6.,1.6));
#7237=CARTESIAN_POINT('',(10.5,6.,1.6));
#7238=CARTESIAN_POINT('',(10.,6.,5.8));
#7239=CARTESIAN_POINT('',(10.,6.,1.6));
#7240=CARTESIAN_POINT('',(10.5,6.,5.8));
#7241=CARTESIAN_POINT('',(10.5,6.,5.8));
#7242=CARTESIAN_POINT('',(10.5,6.,1.6));
#7243=CARTESIAN_POINT('Origin',(10.5,-6.,1.6));
#7244=CARTESIAN_POINT('',(10.5,-6.,1.6));
#7245=CARTESIAN_POINT('',(10.5,-6.,1.6));
#7246=CARTESIAN_POINT('',(10.5,-6.,5.8));
#7247=CARTESIAN_POINT('',(10.5,-6.,5.8));
#7248=CARTESIAN_POINT('',(10.5,-6.,1.6));
#7249=CARTESIAN_POINT('Origin',(10.,-6.,1.6));
#7250=CARTESIAN_POINT('',(10.,-6.,1.6));
#7251=CARTESIAN_POINT('',(10.,-6.,1.6));
#7252=CARTESIAN_POINT('',(10.,-6.,5.8));
#7253=CARTESIAN_POINT('',(10.,-6.,5.8));
#7254=CARTESIAN_POINT('',(10.,-6.,1.6));
#7255=CARTESIAN_POINT('Origin',(10.,6.,1.6));
#7256=CARTESIAN_POINT('',(10.,6.,1.6));
#7257=CARTESIAN_POINT('',(10.,6.,5.8));
#7258=CARTESIAN_POINT('Origin',(10.25,0.,5.8));
#7259=CARTESIAN_POINT('Origin',(10.25,0.,1.6));
#7260=CARTESIAN_POINT('',(0.,0.,0.));
#7261=CARTESIAN_POINT('Origin',(19.4,5.5,3.));
#7262=CARTESIAN_POINT('',(19.5,5.5,3.225));
#7263=CARTESIAN_POINT('Origin',(19.5,5.5,3.));
#7264=CARTESIAN_POINT('',(20.,5.5,3.225));
#7265=CARTESIAN_POINT('',(19.4,5.5,3.225));
#7266=CARTESIAN_POINT('Origin',(20.,5.5,3.));
#7267=CARTESIAN_POINT('Origin',(19.4,-5.5,5.));
#7268=CARTESIAN_POINT('',(19.5,-5.5,5.225));
#7269=CARTESIAN_POINT('Origin',(19.5,-5.5,5.));
#7270=CARTESIAN_POINT('',(20.,-5.5,5.225));
#7271=CARTESIAN_POINT('',(19.4,-5.5,5.225));
#7272=CARTESIAN_POINT('Origin',(20.,-5.5,5.));
#7273=CARTESIAN_POINT('Origin',(19.4,-5.5,3.));
#7274=CARTESIAN_POINT('',(19.5,-5.5,3.225));
#7275=CARTESIAN_POINT('Origin',(19.5,-5.5,3.));
#7276=CARTESIAN_POINT('',(20.,-5.5,3.225));
#7277=CARTESIAN_POINT('',(19.4,-5.5,3.225));
#7278=CARTESIAN_POINT('Origin',(20.,-5.5,3.));
#7279=CARTESIAN_POINT('Origin',(19.4,5.5,5.));
#7280=CARTESIAN_POINT('',(19.5,5.5,5.225));
#7281=CARTESIAN_POINT('Origin',(19.5,5.5,5.));
#7282=CARTESIAN_POINT('',(20.,5.5,5.225));
#7283=CARTESIAN_POINT('',(19.4,5.5,5.225));
#7284=CARTESIAN_POINT('Origin',(20.,5.5,5.));
#7285=CARTESIAN_POINT('Origin',(19.4,-4.,3.3));
#7286=CARTESIAN_POINT('',(19.5,-4.,4.));
#7287=CARTESIAN_POINT('Origin',(19.5,-4.,3.3));
#7288=CARTESIAN_POINT('',(20.,-4.,4.));
#7289=CARTESIAN_POINT('',(19.4,-4.,4.));
#7290=CARTESIAN_POINT('Origin',(20.,-4.,3.3));
#7291=CARTESIAN_POINT('Origin',(19.4,4.,3.3));
#7292=CARTESIAN_POINT('',(19.5,4.,4.));
#7293=CARTESIAN_POINT('Origin',(19.5,4.,3.3));
#7294=CARTESIAN_POINT('',(20.,4.,4.));
#7295=CARTESIAN_POINT('',(19.4,4.,4.));
#7296=CARTESIAN_POINT('Origin',(20.,4.,3.3));
#7297=CARTESIAN_POINT('Origin',(20.,6.,1.6));
#7298=CARTESIAN_POINT('',(20.,6.,1.6));
#7299=CARTESIAN_POINT('',(19.5,6.,1.6));
#7300=CARTESIAN_POINT('',(20.,6.,1.6));
#7301=CARTESIAN_POINT('',(19.5,6.,5.8));
#7302=CARTESIAN_POINT('',(19.5,6.,1.6));
#7303=CARTESIAN_POINT('',(20.,6.,5.8));
#7304=CARTESIAN_POINT('',(20.,6.,5.8));
#7305=CARTESIAN_POINT('',(20.,6.,1.6));
#7306=CARTESIAN_POINT('Origin',(20.,-6.,1.6));
#7307=CARTESIAN_POINT('',(20.,-6.,1.6));
#7308=CARTESIAN_POINT('',(20.,-6.,1.6));
#7309=CARTESIAN_POINT('',(20.,-6.,5.8));
#7310=CARTESIAN_POINT('',(20.,-6.,5.8));
#7311=CARTESIAN_POINT('',(20.,-6.,1.6));
#7312=CARTESIAN_POINT('Origin',(19.5,-6.,1.6));
#7313=CARTESIAN_POINT('',(19.5,-6.,1.6));
#7314=CARTESIAN_POINT('',(19.5,-6.,1.6));
#7315=CARTESIAN_POINT('',(19.5,-6.,5.8));
#7316=CARTESIAN_POINT('',(19.5,-6.,5.8));
#7317=CARTESIAN_POINT('',(19.5,-6.,1.6));
#7318=CARTESIAN_POINT('Origin',(19.5,6.,1.6));
#7319=CARTESIAN_POINT('',(19.5,6.,1.6));
#7320=CARTESIAN_POINT('',(19.5,6.,5.8));
#7321=CARTESIAN_POINT('Origin',(19.75,0.,5.8));
#7322=CARTESIAN_POINT('Origin',(19.75,0.,1.6));
#7323=CARTESIAN_POINT('',(0.,0.,0.));
#7324=CARTESIAN_POINT('Origin',(15.,0.,5.7));
#7325=CARTESIAN_POINT('',(14.75,-3.06161699786838E-17,5.8));
#7326=CARTESIAN_POINT('Origin',(15.,0.,5.8));
#7327=CARTESIAN_POINT('',(14.75,3.06161699786838E-17,6.6));
#7328=CARTESIAN_POINT('',(14.75,-3.06161699786838E-17,5.7));
#7329=CARTESIAN_POINT('Origin',(15.,0.,6.6));
#7330=CARTESIAN_POINT('Origin',(18.5,-1.5,5.7));
#7331=CARTESIAN_POINT('',(18.225,-1.5,5.8));
#7332=CARTESIAN_POINT('Origin',(18.5,-1.5,5.8));
#7333=CARTESIAN_POINT('',(18.225,-1.5,6.6));
#7334=CARTESIAN_POINT('',(18.225,-1.5,5.7));
#7335=CARTESIAN_POINT('Origin',(18.5,-1.5,6.6));
#7336=CARTESIAN_POINT('Origin',(11.5,1.5,5.7));
#7337=CARTESIAN_POINT('',(11.225,1.5,5.8));
#7338=CARTESIAN_POINT('Origin',(11.5,1.5,5.8));
#7339=CARTESIAN_POINT('',(11.225,1.5,6.6));
#7340=CARTESIAN_POINT('',(11.225,1.5,5.7));
#7341=CARTESIAN_POINT('Origin',(11.5,1.5,6.6));
#7342=CARTESIAN_POINT('Origin',(11.5,-1.5,5.7));
#7343=CARTESIAN_POINT('',(11.225,-1.5,5.8));
#7344=CARTESIAN_POINT('Origin',(11.5,-1.5,5.8));
#7345=CARTESIAN_POINT('',(11.225,-1.5,6.6));
#7346=CARTESIAN_POINT('',(11.225,-1.5,5.7));
#7347=CARTESIAN_POINT('Origin',(11.5,-1.5,6.6));
#7348=CARTESIAN_POINT('Origin',(18.5,1.5,5.7));
#7349=CARTESIAN_POINT('',(18.225,1.5,5.8));
#7350=CARTESIAN_POINT('Origin',(18.5,1.5,5.8));
#7351=CARTESIAN_POINT('',(18.225,1.5,6.6));
#7352=CARTESIAN_POINT('',(18.225,1.5,5.7));
#7353=CARTESIAN_POINT('Origin',(18.5,1.5,6.6));
#7354=CARTESIAN_POINT('Origin',(20.5,6.5,5.8));
#7355=CARTESIAN_POINT('',(20.5,6.5,5.8));
#7356=CARTESIAN_POINT('',(9.5,6.5,5.8));
#7357=CARTESIAN_POINT('',(20.5,6.5,5.8));
#7358=CARTESIAN_POINT('',(9.5,6.5,6.6));
#7359=CARTESIAN_POINT('',(9.5,6.5,5.8));
#7360=CARTESIAN_POINT('',(20.5,6.5,6.6));
#7361=CARTESIAN_POINT('',(20.5,6.5,6.6));
#7362=CARTESIAN_POINT('',(20.5,6.5,5.8));
#7363=CARTESIAN_POINT('Origin',(20.5,-6.5,5.8));
#7364=CARTESIAN_POINT('',(20.5,-6.5,5.8));
#7365=CARTESIAN_POINT('',(20.5,-6.5,5.8));
#7366=CARTESIAN_POINT('',(20.5,-6.5,6.6));
#7367=CARTESIAN_POINT('',(20.5,-6.5,6.6));
#7368=CARTESIAN_POINT('',(20.5,-6.5,5.8));
#7369=CARTESIAN_POINT('Origin',(9.5,-6.5,5.8));
#7370=CARTESIAN_POINT('',(9.5,-6.5,5.8));
#7371=CARTESIAN_POINT('',(9.5,-6.5,5.8));
#7372=CARTESIAN_POINT('',(9.5,-6.5,6.6));
#7373=CARTESIAN_POINT('',(9.5,-6.5,6.6));
#7374=CARTESIAN_POINT('',(9.5,-6.5,5.8));
#7375=CARTESIAN_POINT('Origin',(9.5,6.5,5.8));
#7376=CARTESIAN_POINT('',(9.5,6.5,5.8));
#7377=CARTESIAN_POINT('',(9.5,6.5,6.6));
#7378=CARTESIAN_POINT('Origin',(15.,0.,6.6));
#7379=CARTESIAN_POINT('Origin',(15.,0.,5.8));
#7380=CARTESIAN_POINT('',(0.,0.,0.));
#7381=CARTESIAN_POINT('Origin',(15.,0.,6.6));
#7382=CARTESIAN_POINT('',(14.67,-4.04133443718627E-17,8.2));
#7383=CARTESIAN_POINT('Origin',(15.,0.,8.2));
#7384=CARTESIAN_POINT('',(14.67,-4.04133443718627E-17,6.6));
#7385=CARTESIAN_POINT('',(14.67,-4.04133443718627E-17,6.6));
#7386=CARTESIAN_POINT('Origin',(15.,0.,6.6));
#7387=CARTESIAN_POINT('Origin',(15.,0.,6.6));
#7388=CARTESIAN_POINT('',(13.5,-1.83697019872103E-16,8.2));
#7389=CARTESIAN_POINT('Origin',(15.,0.,8.2));
#7390=CARTESIAN_POINT('',(13.5,-1.83697019872103E-16,6.6));
#7391=CARTESIAN_POINT('',(13.5,-1.83697019872103E-16,6.6));
#7392=CARTESIAN_POINT('Origin',(15.,0.,6.6));
#7393=CARTESIAN_POINT('Origin',(15.,0.,8.2));
#7394=CARTESIAN_POINT('Origin',(15.,0.,6.6));
#7395=CARTESIAN_POINT('',(0.,0.,0.));
#7396=CARTESIAN_POINT('',(0.,0.,0.));
#7397=CARTESIAN_POINT('Origin',(0.75,1.2,0.));
#7398=CARTESIAN_POINT('',(0.885663593019381,1.2,-0.16));
#7399=CARTESIAN_POINT('',(0.885663593019381,1.2,0.16));
#7400=CARTESIAN_POINT('Origin',(0.,1.2,0.));
#7401=CARTESIAN_POINT('',(0.93,1.2,-0.16));
#7402=CARTESIAN_POINT('',(0.93,1.2,-0.16));
#7403=CARTESIAN_POINT('',(0.93,1.2,0.16));
#7404=CARTESIAN_POINT('',(0.93,1.2,0.16));
#7405=CARTESIAN_POINT('',(0.57,1.2,0.16));
#7406=CARTESIAN_POINT('Origin',(0.57,0.,0.16));
#7407=CARTESIAN_POINT('',(0.885663593019381,-1.2,0.16));
#7408=CARTESIAN_POINT('',(0.885663593019381,0.,0.16));
#7409=CARTESIAN_POINT('',(0.93,-1.2,0.16));
#7410=CARTESIAN_POINT('',(0.93,0.,0.16));
#7411=CARTESIAN_POINT('',(0.57,-1.2,0.16));
#7412=CARTESIAN_POINT('Origin',(0.75,-1.2,0.));
#7413=CARTESIAN_POINT('',(0.885663593019381,-1.2,-0.16));
#7414=CARTESIAN_POINT('Origin',(0.,-1.2,0.));
#7415=CARTESIAN_POINT('',(0.93,-1.2,-0.16));
#7416=CARTESIAN_POINT('',(0.93,-1.2,0.16));
#7417=CARTESIAN_POINT('',(0.93,-1.2,-0.16));
#7418=CARTESIAN_POINT('Origin',(0.93,0.,-0.16));
#7419=CARTESIAN_POINT('',(0.885663593019381,0.,-0.16));
#7420=CARTESIAN_POINT('',(0.93,0.,-0.16));
#7421=CARTESIAN_POINT('Origin',(0.93,0.,0.16));
#7422=CARTESIAN_POINT('Origin',(1.05,1.5,0.));
#7423=CARTESIAN_POINT('',(-1.05,1.5,-1.28587913910472E-16));
#7424=CARTESIAN_POINT('Origin',(0.,1.5,0.));
#7425=CARTESIAN_POINT('',(-0.9,1.5,-1.10218211923262E-16));
#7426=CARTESIAN_POINT('Origin',(0.,1.5,0.));
#7427=CARTESIAN_POINT('Origin',(0.,1.315,0.));
#7428=CARTESIAN_POINT('',(-1.05,1.13,-1.28587913910472E-16));
#7429=CARTESIAN_POINT('Origin',(0.,1.13,0.));
#7430=CARTESIAN_POINT('',(-1.05,1.315,-1.28587913910472E-16));
#7431=CARTESIAN_POINT('Origin',(1.,1.13,0.));
#7432=CARTESIAN_POINT('',(-1.,1.13,-1.22464679914735E-16));
#7433=CARTESIAN_POINT('Origin',(0.,1.13,0.));
#7434=CARTESIAN_POINT('Origin',(0.,1.065,0.));
#7435=CARTESIAN_POINT('',(-1.,1.,-1.22464679914735E-16));
#7436=CARTESIAN_POINT('Origin',(0.,1.,0.));
#7437=CARTESIAN_POINT('',(-1.,1.065,-1.22464679914735E-16));
#7438=CARTESIAN_POINT('Origin',(1.05,1.,0.));
#7439=CARTESIAN_POINT('',(-1.05,1.,-1.28587913910472E-16));
#7440=CARTESIAN_POINT('Origin',(0.,1.,0.));
#7441=CARTESIAN_POINT('Origin',(0.,0.,0.));
#7442=CARTESIAN_POINT('',(-1.05,-1.,-1.28587913910472E-16));
#7443=CARTESIAN_POINT('Origin',(0.,-1.,0.));
#7444=CARTESIAN_POINT('',(-1.05,0.,-1.28587913910472E-16));
#7445=CARTESIAN_POINT('Origin',(1.,-1.,0.));
#7446=CARTESIAN_POINT('',(-1.,-1.,-1.22464679914735E-16));
#7447=CARTESIAN_POINT('Origin',(0.,-1.,0.));
#7448=CARTESIAN_POINT('Origin',(0.,-1.065,0.));
#7449=CARTESIAN_POINT('',(-1.,-1.13,-1.22464679914735E-16));
#7450=CARTESIAN_POINT('Origin',(0.,-1.13,0.));
#7451=CARTESIAN_POINT('',(-1.,-1.065,-1.22464679914735E-16));
#7452=CARTESIAN_POINT('Origin',(1.05,-1.13,0.));
#7453=CARTESIAN_POINT('',(-1.05,-1.13,-1.28587913910472E-16));
#7454=CARTESIAN_POINT('Origin',(0.,-1.13,0.));
#7455=CARTESIAN_POINT('Origin',(0.,-1.315,0.));
#7456=CARTESIAN_POINT('',(-1.05,-1.5,-1.28587913910472E-16));
#7457=CARTESIAN_POINT('Origin',(0.,-1.5,0.));
#7458=CARTESIAN_POINT('',(-1.05,-1.315,-1.28587913910472E-16));
#7459=CARTESIAN_POINT('Origin',(0.9,-1.5,0.));
#7460=CARTESIAN_POINT('',(-0.9,-1.5,-1.10218211923262E-16));
#7461=CARTESIAN_POINT('Origin',(0.,-1.5,0.));
#7462=CARTESIAN_POINT('Origin',(0.,0.,0.));
#7463=CARTESIAN_POINT('',(-0.9,0.,-1.10218211923262E-16));
#7464=CARTESIAN_POINT('',(0.,0.,0.));
#7465=CARTESIAN_POINT('Origin',(0.75,1.2,0.));
#7466=CARTESIAN_POINT('',(0.880582193778639,1.2,0.16));
#7467=CARTESIAN_POINT('',(0.880582193778639,1.2,-0.16));
#7468=CARTESIAN_POINT('Origin',(0.,1.2,0.));
#7469=CARTESIAN_POINT('',(0.583459510163302,1.2,0.16));
#7470=CARTESIAN_POINT('',(0.57,1.2,0.16));
#7471=CARTESIAN_POINT('',(0.583459510163302,1.2,-0.16));
#7472=CARTESIAN_POINT('Origin',(0.,1.2,0.));
#7473=CARTESIAN_POINT('',(0.93,1.2,-0.16));
#7474=CARTESIAN_POINT('Origin',(0.93,0.,-0.16));
#7475=CARTESIAN_POINT('',(0.880582193778639,-1.2,-0.16));
#7476=CARTESIAN_POINT('',(0.880582193778639,0.,-0.16));
#7477=CARTESIAN_POINT('',(0.583459510163302,-1.2,-0.16));
#7478=CARTESIAN_POINT('',(0.583459510163302,0.,-0.16));
#7479=CARTESIAN_POINT('',(0.93,-1.2,-0.16));
#7480=CARTESIAN_POINT('Origin',(0.75,-1.2,0.));
#7481=CARTESIAN_POINT('',(0.880582193778639,-1.2,0.16));
#7482=CARTESIAN_POINT('Origin',(0.,-1.2,0.));
#7483=CARTESIAN_POINT('',(0.583459510163302,-1.2,0.16));
#7484=CARTESIAN_POINT('Origin',(0.,-1.2,0.));
#7485=CARTESIAN_POINT('',(0.57,-1.2,0.16));
#7486=CARTESIAN_POINT('Origin',(0.57,0.,0.16));
#7487=CARTESIAN_POINT('',(0.880582193778639,0.,0.16));
#7488=CARTESIAN_POINT('',(0.583459510163302,0.,0.16));
#7489=CARTESIAN_POINT('Origin',(0.895,1.35,0.));
#7490=CARTESIAN_POINT('',(-0.895,1.35,-1.09605888523688E-16));
#7491=CARTESIAN_POINT('Origin',(0.,1.35,0.));
#7492=CARTESIAN_POINT('',(-0.605,1.35,-7.40911313484149E-17));
#7493=CARTESIAN_POINT('Origin',(0.,1.35,0.));
#7494=CARTESIAN_POINT('Origin',(0.,0.,0.));
#7495=CARTESIAN_POINT('',(-0.895,-1.35,-1.09605888523688E-16));
#7496=CARTESIAN_POINT('Origin',(0.,-1.35,0.));
#7497=CARTESIAN_POINT('',(-0.895,0.,-1.09605888523688E-16));
#7498=CARTESIAN_POINT('Origin',(0.605,-1.35,0.));
#7499=CARTESIAN_POINT('',(-0.605,-1.35,-7.40911313484149E-17));
#7500=CARTESIAN_POINT('Origin',(0.,-1.35,0.));
#7501=CARTESIAN_POINT('Origin',(0.,0.,0.));
#7502=CARTESIAN_POINT('',(-0.605,0.,-7.40911313484149E-17));
#7503=CARTESIAN_POINT('',(0.,0.,0.));
#7504=CARTESIAN_POINT('',(0.,0.,0.));
#7505=CARTESIAN_POINT('',(0.,0.,0.));
#7506=CARTESIAN_POINT('Origin',(0.3,0.4,0.));
#7507=CARTESIAN_POINT('',(-0.3,0.4,-3.67394039744206E-17));
#7508=CARTESIAN_POINT('Origin',(0.,0.4,0.));
#7509=CARTESIAN_POINT('Origin',(0.,0.375,0.));
#7510=CARTESIAN_POINT('',(-0.35,0.35,-4.28626379701573E-17));
#7511=CARTESIAN_POINT('Origin',(0.,0.35,0.));
#7512=CARTESIAN_POINT('',(-0.325,0.375,-3.9801020972289E-17));
#7513=CARTESIAN_POINT('Origin',(0.,0.19,0.));
#7514=CARTESIAN_POINT('',(-0.35,0.03,-4.28626379701574E-17));
#7515=CARTESIAN_POINT('Origin',(0.,0.03,0.));
#7516=CARTESIAN_POINT('',(-0.35,0.19,-4.28626379701574E-17));
#7517=CARTESIAN_POINT('Origin',(0.,0.0149999999999999,0.));
#7518=CARTESIAN_POINT('',(-0.32,-3.29597460435593E-17,-3.91886975727153E-17));
#7519=CARTESIAN_POINT('Origin',(0.,0.,0.));
#7520=CARTESIAN_POINT('',(-0.335,0.0149999999999999,-4.10256677714363E-17));
#7521=CARTESIAN_POINT('Origin',(0.22,0.,0.));
#7522=CARTESIAN_POINT('',(-0.22,-6.93889390390723E-18,-2.69422295812418E-17));
#7523=CARTESIAN_POINT('Origin',(0.,0.,0.));
#7524=CARTESIAN_POINT('Origin',(0.,-0.02,0.));
#7525=CARTESIAN_POINT('',(-0.1954,-0.0492,2.39295984553393E-17));
#7526=CARTESIAN_POINT('Origin',(0.,-0.0492,0.));
#7527=CARTESIAN_POINT('',(-0.21,-0.02,-2.57175827820944E-17));
#7528=CARTESIAN_POINT('Origin',(0.,-0.8,0.));
#7529=CARTESIAN_POINT('',(-0.1954,-1.5646,2.39295984553393E-17));
#7530=CARTESIAN_POINT('Origin',(0.,-1.5646,0.));
#7531=CARTESIAN_POINT('',(-0.1954,-0.8,-2.39295984553393E-17));
#7532=CARTESIAN_POINT('Origin',(0.,-1.58,0.));
#7533=CARTESIAN_POINT('',(-0.16,-1.6,-1.95943487863577E-17));
#7534=CARTESIAN_POINT('Origin',(0.,-1.6,0.));
#7535=CARTESIAN_POINT('',(-0.18,-1.58,-2.20436423846524E-17));
#7536=CARTESIAN_POINT('Origin',(0.,-1.6,0.));
#7537=CARTESIAN_POINT('Origin',(0.0866025403784439,-0.4,-0.15));
#7538=CARTESIAN_POINT('',(0.173205080756888,-0.4,0.));
#7539=CARTESIAN_POINT('',(0.0866025403784439,-0.4,-0.15));
#7540=CARTESIAN_POINT('',(0.173205080756888,-0.4,0.));
#7541=CARTESIAN_POINT('',(0.0866025403784439,-0.64,-0.15));
#7542=CARTESIAN_POINT('',(0.0866025403784439,-0.4,-0.15));
#7543=CARTESIAN_POINT('',(0.173205080756888,-0.64,0.));
#7544=CARTESIAN_POINT('',(0.173205080756888,-0.64,0.));
#7545=CARTESIAN_POINT('',(0.173205080756888,-0.4,0.));
#7546=CARTESIAN_POINT('Origin',(-0.0866025403784438,-0.4,-0.15));
#7547=CARTESIAN_POINT('',(-0.0866025403784438,-0.4,-0.15));
#7548=CARTESIAN_POINT('',(0.0866025403784439,-0.4,-0.15));
#7549=CARTESIAN_POINT('',(-0.0866025403784438,-0.64,-0.15));
#7550=CARTESIAN_POINT('',(-0.0866025403784438,-0.4,-0.15));
#7551=CARTESIAN_POINT('',(0.0866025403784439,-0.64,-0.15));
#7552=CARTESIAN_POINT('Origin',(-0.173205080756888,-0.4,-2.77555756156289E-17));
#7553=CARTESIAN_POINT('',(-0.173205080756888,-0.4,-2.12115047744981E-17));
#7554=CARTESIAN_POINT('',(-0.0866025403784438,-0.4,-0.15));
#7555=CARTESIAN_POINT('',(-0.173205080756888,-0.64,-2.77555756156289E-17));
#7556=CARTESIAN_POINT('',(-0.173205080756888,-0.4,-2.12115047744981E-17));
#7557=CARTESIAN_POINT('',(-0.0866025403784438,-0.64,-0.15));
#7558=CARTESIAN_POINT('Origin',(-0.0866025403784439,-0.4,0.15));
#7559=CARTESIAN_POINT('',(-0.0866025403784439,-0.4,0.15));
#7560=CARTESIAN_POINT('',(-0.173205080756888,-0.4,-2.12115047744981E-17));
#7561=CARTESIAN_POINT('',(-0.0866025403784439,-0.64,0.15));
#7562=CARTESIAN_POINT('',(-0.0866025403784439,-0.4,0.15));
#7563=CARTESIAN_POINT('',(-0.173205080756888,-0.64,-2.12115047744981E-17));
#7564=CARTESIAN_POINT('Origin',(0.0866025403784439,-0.4,0.15));
#7565=CARTESIAN_POINT('',(0.0866025403784439,-0.4,0.15));
#7566=CARTESIAN_POINT('',(-0.0866025403784439,-0.4,0.15));
#7567=CARTESIAN_POINT('',(0.0866025403784439,-0.64,0.15));
#7568=CARTESIAN_POINT('',(0.0866025403784439,-0.4,0.15));
#7569=CARTESIAN_POINT('',(-0.0866025403784439,-0.64,0.15));
#7570=CARTESIAN_POINT('Origin',(0.173205080756888,-0.4,0.));
#7571=CARTESIAN_POINT('',(0.0866025403784439,-0.4,0.15));
#7572=CARTESIAN_POINT('',(0.0866025403784439,-0.64,0.15));
#7573=CARTESIAN_POINT('Origin',(0.,-0.4,-2.77555756156289E-17));
#7574=CARTESIAN_POINT('Origin',(0.,-0.64,-2.77555756156289E-17));
#7575=CARTESIAN_POINT('',(0.,0.,0.));
#7576=CARTESIAN_POINT('Origin',(0.375,0.5,0.));
#7577=CARTESIAN_POINT('',(-0.375,0.5,-4.59242549680257E-17));
#7578=CARTESIAN_POINT('Origin',(0.,0.5,0.));
#7579=CARTESIAN_POINT('Origin',(0.,0.475,0.));
#7580=CARTESIAN_POINT('',(-0.425,0.45,-5.20474889637625E-17));
#7581=CARTESIAN_POINT('Origin',(0.,0.45,0.));
#7582=CARTESIAN_POINT('',(-0.4,0.475,-4.89858719658941E-17));
#7583=CARTESIAN_POINT('Origin',(0.,0.24,0.));
#7584=CARTESIAN_POINT('',(-0.425,0.0299999999999998,-5.20474889637625E-17));
#7585=CARTESIAN_POINT('Origin',(0.,0.0299999999999998,0.));
#7586=CARTESIAN_POINT('',(-0.425,0.24,-5.20474889637625E-17));
#7587=CARTESIAN_POINT('Origin',(0.,0.0150000000000001,0.));
#7588=CARTESIAN_POINT('',(-0.395,4.85722573273506E-17,-4.83735485663204E-17));
#7589=CARTESIAN_POINT('Origin',(0.,0.,0.));
#7590=CARTESIAN_POINT('',(-0.41,0.0150000000000001,-5.02105187650415E-17));
#7591=CARTESIAN_POINT('Origin',(0.27,0.,0.));
#7592=CARTESIAN_POINT('',(-0.27,0.,-3.30654635769785E-17));
#7593=CARTESIAN_POINT('Origin',(0.,0.,0.));
#7594=CARTESIAN_POINT('Origin',(0.,-0.02,0.));
#7595=CARTESIAN_POINT('',(-0.24505,-0.0498999999999999,3.00099698131059E-17));
#7596=CARTESIAN_POINT('Origin',(0.,-0.0498999999999999,0.));
#7597=CARTESIAN_POINT('',(-0.26,-0.02,-3.18408167778312E-17));
#7598=CARTESIAN_POINT('Origin',(0.,-0.995,0.));
#7599=CARTESIAN_POINT('',(-0.24505,-1.95495,3.00099698131059E-17));
#7600=CARTESIAN_POINT('Origin',(0.,-1.95495,0.));
#7601=CARTESIAN_POINT('',(-0.24505,-0.995,-3.00099698131059E-17));
#7602=CARTESIAN_POINT('Origin',(0.,-1.975,0.));
#7603=CARTESIAN_POINT('',(-0.2,-2.,-2.44929359829471E-17));
#7604=CARTESIAN_POINT('Origin',(0.,-2.,0.));
#7605=CARTESIAN_POINT('',(-0.225,-1.975,-2.75545529808154E-17));
#7606=CARTESIAN_POINT('Origin',(0.,-2.,0.));
#7607=CARTESIAN_POINT('Origin',(0.115470053837925,-0.5,-0.2));
#7608=CARTESIAN_POINT('',(0.23094010767585,-0.5,0.));
#7609=CARTESIAN_POINT('',(0.115470053837925,-0.5,-0.2));
#7610=CARTESIAN_POINT('',(0.23094010767585,-0.5,0.));
#7611=CARTESIAN_POINT('',(0.115470053837925,-0.8,-0.2));
#7612=CARTESIAN_POINT('',(0.115470053837925,-0.5,-0.2));
#7613=CARTESIAN_POINT('',(0.23094010767585,-0.8,0.));
#7614=CARTESIAN_POINT('',(0.23094010767585,-0.8,0.));
#7615=CARTESIAN_POINT('',(0.23094010767585,-0.5,0.));
#7616=CARTESIAN_POINT('Origin',(-0.115470053837925,-0.5,-0.2));
#7617=CARTESIAN_POINT('',(-0.115470053837925,-0.5,-0.2));
#7618=CARTESIAN_POINT('',(0.115470053837925,-0.5,-0.2));
#7619=CARTESIAN_POINT('',(-0.115470053837925,-0.8,-0.2));
#7620=CARTESIAN_POINT('',(-0.115470053837925,-0.5,-0.2));
#7621=CARTESIAN_POINT('',(0.115470053837925,-0.8,-0.2));
#7622=CARTESIAN_POINT('Origin',(-0.23094010767585,-0.5,-2.77555756156289E-17));
#7623=CARTESIAN_POINT('',(-0.23094010767585,-0.5,-2.82820063659975E-17));
#7624=CARTESIAN_POINT('',(-0.115470053837925,-0.5,-0.2));
#7625=CARTESIAN_POINT('',(-0.23094010767585,-0.8,-2.77555756156289E-17));
#7626=CARTESIAN_POINT('',(-0.23094010767585,-0.5,-2.82820063659975E-17));
#7627=CARTESIAN_POINT('',(-0.115470053837925,-0.8,-0.2));
#7628=CARTESIAN_POINT('Origin',(-0.115470053837925,-0.5,0.2));
#7629=CARTESIAN_POINT('',(-0.115470053837925,-0.5,0.2));
#7630=CARTESIAN_POINT('',(-0.23094010767585,-0.5,-2.82820063659975E-17));
#7631=CARTESIAN_POINT('',(-0.115470053837925,-0.8,0.2));
#7632=CARTESIAN_POINT('',(-0.115470053837925,-0.5,0.2));
#7633=CARTESIAN_POINT('',(-0.23094010767585,-0.8,-2.82820063659975E-17));
#7634=CARTESIAN_POINT('Origin',(0.115470053837925,-0.5,0.2));
#7635=CARTESIAN_POINT('',(0.115470053837925,-0.5,0.2));
#7636=CARTESIAN_POINT('',(-0.115470053837925,-0.5,0.2));
#7637=CARTESIAN_POINT('',(0.115470053837925,-0.8,0.2));
#7638=CARTESIAN_POINT('',(0.115470053837925,-0.5,0.2));
#7639=CARTESIAN_POINT('',(-0.115470053837925,-0.8,0.2));
#7640=CARTESIAN_POINT('Origin',(0.23094010767585,-0.5,0.));
#7641=CARTESIAN_POINT('',(0.115470053837925,-0.5,0.2));
#7642=CARTESIAN_POINT('',(0.115470053837925,-0.8,0.2));
#7643=CARTESIAN_POINT('Origin',(0.,-0.5,0.));
#7644=CARTESIAN_POINT('Origin',(0.,-0.8,0.));
#7645=CARTESIAN_POINT('',(0.,0.,0.));
#7646=CARTESIAN_POINT('',(0.,0.,0.));
#7647=CARTESIAN_POINT('',(0.,0.,0.));
#7648=CARTESIAN_POINT('',(0.,0.,0.));
#7649=CARTESIAN_POINT('',(0.,0.,0.));
#7650=CARTESIAN_POINT('',(0.,-4.,3.3));
#7651=CARTESIAN_POINT('',(1.,-4.,1.));
#7652=CARTESIAN_POINT('',(1.,-5.6,1.6));
#7653=CARTESIAN_POINT('',(1.,-2.4,1.6));
#7654=CARTESIAN_POINT('',(1.,-5.2,4.35));
#7655=CARTESIAN_POINT('',(29.,-4.,1.));
#7656=CARTESIAN_POINT('',(29.,-5.6,1.6));
#7657=CARTESIAN_POINT('',(29.,-2.4,1.6));
#7658=CARTESIAN_POINT('',(29.,-5.2,4.35));
#7659=CARTESIAN_POINT('',(0.,4.,3.3));
#7660=CARTESIAN_POINT('',(1.,4.,1.));
#7661=CARTESIAN_POINT('',(1.,2.4,1.6));
#7662=CARTESIAN_POINT('',(1.,5.6,1.6));
#7663=CARTESIAN_POINT('',(1.,2.8,4.35));
#7664=CARTESIAN_POINT('',(29.,4.,1.));
#7665=CARTESIAN_POINT('',(29.,2.4,1.6));
#7666=CARTESIAN_POINT('',(29.,5.6,1.6));
#7667=CARTESIAN_POINT('',(29.,2.8,4.35));
#7668=CARTESIAN_POINT('',(3.5,-5.5,2.));
#7669=CARTESIAN_POINT('',(3.5,5.5,2.));
#7670=CARTESIAN_POINT('',(26.5,-5.5,2.));
#7671=CARTESIAN_POINT('',(26.5,5.5,2.));
#7672=CARTESIAN_POINT('',(0.,0.,0.));
#7673=CARTESIAN_POINT('Origin',(0.,0.,0.));
#7674=CARTESIAN_POINT('',(-0.32,0.16,3.91886975727153E-17));
#7675=CARTESIAN_POINT('Origin',(0.,0.16,0.));
#7676=CARTESIAN_POINT('',(-0.32,0.,3.91886975727153E-17));
#7677=CARTESIAN_POINT('',(-0.32,0.,3.91886975727153E-17));
#7678=CARTESIAN_POINT('Origin',(0.,0.,0.));
#7679=CARTESIAN_POINT('Origin',(0.,0.,0.));
#7680=CARTESIAN_POINT('',(-0.6,0.16,7.34788079488412E-17));
#7681=CARTESIAN_POINT('Origin',(0.,0.16,0.));
#7682=CARTESIAN_POINT('',(-0.6,0.,7.34788079488412E-17));
#7683=CARTESIAN_POINT('',(-0.6,0.,7.34788079488412E-17));
#7684=CARTESIAN_POINT('Origin',(0.,0.,0.));
#7685=CARTESIAN_POINT('Origin',(0.,0.16,0.));
#7686=CARTESIAN_POINT('Origin',(0.,0.,0.));
#7687=CARTESIAN_POINT('',(0.,0.,0.));
#7688=CARTESIAN_POINT('Origin',(0.45,0.6,0.));
#7689=CARTESIAN_POINT('',(-0.45,0.6,-5.51091059616309E-17));
#7690=CARTESIAN_POINT('Origin',(0.,0.6,0.));
#7691=CARTESIAN_POINT('Origin',(0.,0.575,0.));
#7692=CARTESIAN_POINT('',(-0.5,0.55,-6.12323399573677E-17));
#7693=CARTESIAN_POINT('Origin',(0.,0.55,0.));
#7694=CARTESIAN_POINT('',(-0.475,0.575,-5.81707229594993E-17));
#7695=CARTESIAN_POINT('Origin',(0.,0.29,0.));
#7696=CARTESIAN_POINT('',(-0.5,0.0299999999999998,-6.12323399573677E-17));
#7697=CARTESIAN_POINT('Origin',(0.,0.0299999999999998,0.));
#7698=CARTESIAN_POINT('',(-0.5,0.29,-6.12323399573677E-17));
#7699=CARTESIAN_POINT('Origin',(0.,0.0150000000000001,0.));
#7700=CARTESIAN_POINT('',(-0.47,7.11236625150491E-17,-5.75583995599256E-17));
#7701=CARTESIAN_POINT('Origin',(0.,0.,0.));
#7702=CARTESIAN_POINT('',(-0.485,0.0150000000000001,-5.93953697586466E-17));
#7703=CARTESIAN_POINT('Origin',(0.32,0.,0.));
#7704=CARTESIAN_POINT('',(-0.32,-6.93889390390723E-18,-3.91886975727153E-17));
#7705=CARTESIAN_POINT('Origin',(0.,0.,0.));
#7706=CARTESIAN_POINT('Origin',(0.,-0.02,0.));
#7707=CARTESIAN_POINT('',(-0.2942,-0.0515999999999999,3.60291088309151E-17));
#7708=CARTESIAN_POINT('Origin',(0.,-0.0515999999999999,0.));
#7709=CARTESIAN_POINT('',(-0.31,-0.02,-3.7964050773568E-17));
#7710=CARTESIAN_POINT('Origin',(0.,-1.24,0.));
#7711=CARTESIAN_POINT('',(-0.2942,-2.4458,3.60291088309151E-17));
#7712=CARTESIAN_POINT('Origin',(0.,-2.4458,0.));
#7713=CARTESIAN_POINT('',(-0.2942,-1.24,-3.60291088309151E-17));
#7714=CARTESIAN_POINT('Origin',(0.,-2.47,0.));
#7715=CARTESIAN_POINT('',(-0.24,-2.5,-2.93915231795365E-17));
#7716=CARTESIAN_POINT('Origin',(0.,-2.5,0.));
#7717=CARTESIAN_POINT('',(-0.27,-2.47,-3.30654635769785E-17));
#7718=CARTESIAN_POINT('Origin',(0.,-2.5,0.));
#7719=CARTESIAN_POINT('Origin',(0.144337567297406,-0.6,-0.25));
#7720=CARTESIAN_POINT('',(0.288675134594813,-0.6,0.));
#7721=CARTESIAN_POINT('',(0.144337567297406,-0.6,-0.25));
#7722=CARTESIAN_POINT('',(0.288675134594813,-0.6,0.));
#7723=CARTESIAN_POINT('',(0.144337567297406,-0.96,-0.25));
#7724=CARTESIAN_POINT('',(0.144337567297406,-0.6,-0.25));
#7725=CARTESIAN_POINT('',(0.288675134594813,-0.96,0.));
#7726=CARTESIAN_POINT('',(0.288675134594813,-0.96,0.));
#7727=CARTESIAN_POINT('',(0.288675134594813,-0.6,0.));
#7728=CARTESIAN_POINT('Origin',(-0.144337567297406,-0.6,-0.25));
#7729=CARTESIAN_POINT('',(-0.144337567297406,-0.6,-0.25));
#7730=CARTESIAN_POINT('',(0.144337567297406,-0.6,-0.25));
#7731=CARTESIAN_POINT('',(-0.144337567297406,-0.96,-0.25));
#7732=CARTESIAN_POINT('',(-0.144337567297406,-0.6,-0.25));
#7733=CARTESIAN_POINT('',(0.144337567297406,-0.96,-0.25));
#7734=CARTESIAN_POINT('Origin',(-0.288675134594813,-0.6,-8.32667268468867E-17));
#7735=CARTESIAN_POINT('',(-0.288675134594813,-0.6,-3.53525079574969E-17));
#7736=CARTESIAN_POINT('',(-0.144337567297406,-0.6,-0.25));
#7737=CARTESIAN_POINT('',(-0.288675134594813,-0.96,-5.55111512312578E-17));
#7738=CARTESIAN_POINT('',(-0.288675134594813,-0.6,-3.53525079574969E-17));
#7739=CARTESIAN_POINT('',(-0.144337567297406,-0.96,-0.25));
#7740=CARTESIAN_POINT('Origin',(-0.144337567297407,-0.6,0.25));
#7741=CARTESIAN_POINT('',(-0.144337567297407,-0.6,0.25));
#7742=CARTESIAN_POINT('',(-0.288675134594813,-0.6,-3.53525079574969E-17));
#7743=CARTESIAN_POINT('',(-0.144337567297407,-0.96,0.25));
#7744=CARTESIAN_POINT('',(-0.144337567297407,-0.6,0.25));
#7745=CARTESIAN_POINT('',(-0.288675134594813,-0.96,-3.53525079574969E-17));
#7746=CARTESIAN_POINT('Origin',(0.144337567297406,-0.6,0.25));
#7747=CARTESIAN_POINT('',(0.144337567297406,-0.6,0.25));
#7748=CARTESIAN_POINT('',(-0.144337567297407,-0.6,0.25));
#7749=CARTESIAN_POINT('',(0.144337567297406,-0.96,0.25));
#7750=CARTESIAN_POINT('',(0.144337567297406,-0.6,0.25));
#7751=CARTESIAN_POINT('',(-0.144337567297407,-0.96,0.25));
#7752=CARTESIAN_POINT('Origin',(0.288675134594813,-0.6,0.));
#7753=CARTESIAN_POINT('',(0.144337567297406,-0.6,0.25));
#7754=CARTESIAN_POINT('',(0.144337567297406,-0.96,0.25));
#7755=CARTESIAN_POINT('Origin',(0.,-0.6,0.));
#7756=CARTESIAN_POINT('Origin',(0.,-0.96,0.));
#7757=CARTESIAN_POINT('',(0.,0.,0.));
#7758=CARTESIAN_POINT('',(0.,0.,0.));
#7759=CARTESIAN_POINT('',(0.,0.,0.));
#7760=CARTESIAN_POINT('',(0.,0.,0.));
#7761=CARTESIAN_POINT('',(0.,0.,0.));
#7762=CARTESIAN_POINT('',(0.,0.,0.));
#7763=CARTESIAN_POINT('',(0.,0.,0.));
#7764=CARTESIAN_POINT('',(12.,-4.,3.3));
#7765=CARTESIAN_POINT('',(18.,-4.,3.3));
#7766=CARTESIAN_POINT('',(12.,4.,3.3));
#7767=CARTESIAN_POINT('',(18.,4.,3.3));
#7768=CARTESIAN_POINT('',(10.,-5.5,3.));
#7769=CARTESIAN_POINT('',(10.,-5.5,5.));
#7770=CARTESIAN_POINT('',(10.,5.5,3.));
#7771=CARTESIAN_POINT('',(10.,5.5,5.));
#7772=CARTESIAN_POINT('',(20.,-5.5,3.));
#7773=CARTESIAN_POINT('',(20.,-5.5,5.));
#7774=CARTESIAN_POINT('',(20.,5.5,3.));
#7775=CARTESIAN_POINT('',(20.,5.5,5.));
#7776=CARTESIAN_POINT('',(11.5,-1.5,6.6));
#7777=CARTESIAN_POINT('',(11.5,1.5,6.6));
#7778=CARTESIAN_POINT('',(18.5,-1.5,6.6));
#7779=CARTESIAN_POINT('',(18.5,1.5,6.6));
#7780=CARTESIAN_POINT('',(15.,0.,8.2));
#7781=CARTESIAN_POINT('',(15.,0.,8.36));
#7782=CARTESIAN_POINT('',(0.,0.,0.));
#7783=CARTESIAN_POINT('',(0.,0.,0.));
#7784=UNCERTAINTY_MEASURE_WITH_UNIT(LENGTH_MEASURE(0.001),#7836,
'DISTANCE_ACCURACY_VALUE',
'Maximum model space distance between geometric entities at asserted c
onnectivities');
#7785=UNCERTAINTY_MEASURE_WITH_UNIT(LENGTH_MEASURE(0.001),#7836,
'DISTANCE_ACCURACY_VALUE',
'Maximum model space distance between geometric entities at asserted c
onnectivities');
#7786=UNCERTAINTY_MEASURE_WITH_UNIT(LENGTH_MEASURE(0.001),#7836,
'DISTANCE_ACCURACY_VALUE',
'Maximum model space distance between geometric entities at asserted c
onnectivities');
#7787=UNCERTAINTY_MEASURE_WITH_UNIT(LENGTH_MEASURE(0.001),#7836,
'DISTANCE_ACCURACY_VALUE',
'Maximum model space distance between geometric entities at asserted c
onnectivities');
#7788=UNCERTAINTY_MEASURE_WITH_UNIT(LENGTH_MEASURE(0.001),#7836,
'DISTANCE_ACCURACY_VALUE',
'Maximum model space distance between geometric entities at asserted c
onnectivities');
#7789=UNCERTAINTY_MEASURE_WITH_UNIT(LENGTH_MEASURE(0.001),#7836,
'DISTANCE_ACCURACY_VALUE',
'Maximum model space distance between geometric entities at asserted c
onnectivities');
#7790=UNCERTAINTY_MEASURE_WITH_UNIT(LENGTH_MEASURE(0.001),#7836,
'DISTANCE_ACCURACY_VALUE',
'Maximum model space distance between geometric entities at asserted c
onnectivities');
#7791=UNCERTAINTY_MEASURE_WITH_UNIT(LENGTH_MEASURE(0.001),#7836,
'DISTANCE_ACCURACY_VALUE',
'Maximum model space distance between geometric entities at asserted c
onnectivities');
#7792=UNCERTAINTY_MEASURE_WITH_UNIT(LENGTH_MEASURE(0.001),#7836,
'DISTANCE_ACCURACY_VALUE',
'Maximum model space distance between geometric entities at asserted c
onnectivities');
#7793=UNCERTAINTY_MEASURE_WITH_UNIT(LENGTH_MEASURE(0.001),#7836,
'DISTANCE_ACCURACY_VALUE',
'Maximum model space distance between geometric entities at asserted c
onnectivities');
#7794=UNCERTAINTY_MEASURE_WITH_UNIT(LENGTH_MEASURE(0.001),#7836,
'DISTANCE_ACCURACY_VALUE',
'Maximum model space distance between geometric entities at asserted c
onnectivities');
#7795=UNCERTAINTY_MEASURE_WITH_UNIT(LENGTH_MEASURE(0.001),#7836,
'DISTANCE_ACCURACY_VALUE',
'Maximum model space distance between geometric entities at asserted c
onnectivities');
#7796=UNCERTAINTY_MEASURE_WITH_UNIT(LENGTH_MEASURE(0.001),#7836,
'DISTANCE_ACCURACY_VALUE',
'Maximum model space distance between geometric entities at asserted c
onnectivities');
#7797=UNCERTAINTY_MEASURE_WITH_UNIT(LENGTH_MEASURE(0.001),#7836,
'DISTANCE_ACCURACY_VALUE',
'Maximum model space distance between geometric entities at asserted c
onnectivities');
#7798=UNCERTAINTY_MEASURE_WITH_UNIT(LENGTH_MEASURE(0.001),#7836,
'DISTANCE_ACCURACY_VALUE',
'Maximum model space distance between geometric entities at asserted c
onnectivities');
#7799=UNCERTAINTY_MEASURE_WITH_UNIT(LENGTH_MEASURE(0.001),#7836,
'DISTANCE_ACCURACY_VALUE',
'Maximum model space distance between geometric entities at asserted c
onnectivities');
#7800=UNCERTAINTY_MEASURE_WITH_UNIT(LENGTH_MEASURE(0.001),#7836,
'DISTANCE_ACCURACY_VALUE',
'Maximum model space distance between geometric entities at asserted c
onnectivities');
#7801=UNCERTAINTY_MEASURE_WITH_UNIT(LENGTH_MEASURE(0.001),#7836,
'DISTANCE_ACCURACY_VALUE',
'Maximum model space distance between geometric entities at asserted c
onnectivities');
#7802=UNCERTAINTY_MEASURE_WITH_UNIT(LENGTH_MEASURE(0.001),#7836,
'DISTANCE_ACCURACY_VALUE',
'Maximum model space distance between geometric entities at asserted c
onnectivities');
#7803=UNCERTAINTY_MEASURE_WITH_UNIT(LENGTH_MEASURE(0.001),#7836,
'DISTANCE_ACCURACY_VALUE',
'Maximum model space distance between geometric entities at asserted c
onnectivities');
#7804=UNCERTAINTY_MEASURE_WITH_UNIT(LENGTH_MEASURE(0.001),#7836,
'DISTANCE_ACCURACY_VALUE',
'Maximum model space distance between geometric entities at asserted c
onnectivities');
#7805=UNCERTAINTY_MEASURE_WITH_UNIT(LENGTH_MEASURE(0.001),#7836,
'DISTANCE_ACCURACY_VALUE',
'Maximum model space distance between geometric entities at asserted c
onnectivities');
#7806=UNCERTAINTY_MEASURE_WITH_UNIT(LENGTH_MEASURE(0.001),#7836,
'DISTANCE_ACCURACY_VALUE',
'Maximum model space distance between geometric entities at asserted c
onnectivities');
#7807=UNCERTAINTY_MEASURE_WITH_UNIT(LENGTH_MEASURE(0.001),#7836,
'DISTANCE_ACCURACY_VALUE',
'Maximum model space distance between geometric entities at asserted c
onnectivities');
#7808=UNCERTAINTY_MEASURE_WITH_UNIT(LENGTH_MEASURE(0.001),#7836,
'DISTANCE_ACCURACY_VALUE',
'Maximum model space distance between geometric entities at asserted c
onnectivities');
#7809=UNCERTAINTY_MEASURE_WITH_UNIT(LENGTH_MEASURE(0.001),#7836,
'DISTANCE_ACCURACY_VALUE',
'Maximum model space distance between geometric entities at asserted c
onnectivities');
#7810=(
GEOMETRIC_REPRESENTATION_CONTEXT(3)
GLOBAL_UNCERTAINTY_ASSIGNED_CONTEXT((#7784))
GLOBAL_UNIT_ASSIGNED_CONTEXT((#7836,#7838,#7839))
REPRESENTATION_CONTEXT('','3D')
);
#7811=(
GEOMETRIC_REPRESENTATION_CONTEXT(3)
GLOBAL_UNCERTAINTY_ASSIGNED_CONTEXT((#7785))
GLOBAL_UNIT_ASSIGNED_CONTEXT((#7836,#7838,#7839))
REPRESENTATION_CONTEXT('','3D')
);
#7812=(
GEOMETRIC_REPRESENTATION_CONTEXT(3)
GLOBAL_UNCERTAINTY_ASSIGNED_CONTEXT((#7786))
GLOBAL_UNIT_ASSIGNED_CONTEXT((#7836,#7838,#7839))
REPRESENTATION_CONTEXT('','3D')
);
#7813=(
GEOMETRIC_REPRESENTATION_CONTEXT(3)
GLOBAL_UNCERTAINTY_ASSIGNED_CONTEXT((#7787))
GLOBAL_UNIT_ASSIGNED_CONTEXT((#7836,#7838,#7839))
REPRESENTATION_CONTEXT('','3D')
);
#7814=(
GEOMETRIC_REPRESENTATION_CONTEXT(3)
GLOBAL_UNCERTAINTY_ASSIGNED_CONTEXT((#7788))
GLOBAL_UNIT_ASSIGNED_CONTEXT((#7836,#7838,#7839))
REPRESENTATION_CONTEXT('','3D')
);
#7815=(
GEOMETRIC_REPRESENTATION_CONTEXT(3)
GLOBAL_UNCERTAINTY_ASSIGNED_CONTEXT((#7789))
GLOBAL_UNIT_ASSIGNED_CONTEXT((#7836,#7838,#7839))
REPRESENTATION_CONTEXT('','3D')
);
#7816=(
GEOMETRIC_REPRESENTATION_CONTEXT(3)
GLOBAL_UNCERTAINTY_ASSIGNED_CONTEXT((#7790))
GLOBAL_UNIT_ASSIGNED_CONTEXT((#7836,#7838,#7839))
REPRESENTATION_CONTEXT('','3D')
);
#7817=(
GEOMETRIC_REPRESENTATION_CONTEXT(3)
GLOBAL_UNCERTAINTY_ASSIGNED_CONTEXT((#7791))
GLOBAL_UNIT_ASSIGNED_CONTEXT((#7836,#7838,#7839))
REPRESENTATION_CONTEXT('','3D')
);
#7818=(
GEOMETRIC_REPRESENTATION_CONTEXT(3)
GLOBAL_UNCERTAINTY_ASSIGNED_CONTEXT((#7792))
GLOBAL_UNIT_ASSIGNED_CONTEXT((#7836,#7838,#7839))
REPRESENTATION_CONTEXT('','3D')
);
#7819=(
GEOMETRIC_REPRESENTATION_CONTEXT(3)
GLOBAL_UNCERTAINTY_ASSIGNED_CONTEXT((#7793))
GLOBAL_UNIT_ASSIGNED_CONTEXT((#7836,#7838,#7839))
REPRESENTATION_CONTEXT('','3D')
);
#7820=(
GEOMETRIC_REPRESENTATION_CONTEXT(3)
GLOBAL_UNCERTAINTY_ASSIGNED_CONTEXT((#7794))
GLOBAL_UNIT_ASSIGNED_CONTEXT((#7836,#7838,#7839))
REPRESENTATION_CONTEXT('','3D')
);
#7821=(
GEOMETRIC_REPRESENTATION_CONTEXT(3)
GLOBAL_UNCERTAINTY_ASSIGNED_CONTEXT((#7795))
GLOBAL_UNIT_ASSIGNED_CONTEXT((#7836,#7838,#7839))
REPRESENTATION_CONTEXT('','3D')
);
#7822=(
GEOMETRIC_REPRESENTATION_CONTEXT(3)
GLOBAL_UNCERTAINTY_ASSIGNED_CONTEXT((#7796))
GLOBAL_UNIT_ASSIGNED_CONTEXT((#7836,#7838,#7839))
REPRESENTATION_CONTEXT('','3D')
);
#7823=(
GEOMETRIC_REPRESENTATION_CONTEXT(3)
GLOBAL_UNCERTAINTY_ASSIGNED_CONTEXT((#7797))
GLOBAL_UNIT_ASSIGNED_CONTEXT((#7836,#7838,#7839))
REPRESENTATION_CONTEXT('','3D')
);
#7824=(
GEOMETRIC_REPRESENTATION_CONTEXT(3)
GLOBAL_UNCERTAINTY_ASSIGNED_CONTEXT((#7798))
GLOBAL_UNIT_ASSIGNED_CONTEXT((#7836,#7838,#7839))
REPRESENTATION_CONTEXT('','3D')
);
#7825=(
GEOMETRIC_REPRESENTATION_CONTEXT(3)
GLOBAL_UNCERTAINTY_ASSIGNED_CONTEXT((#7799))
GLOBAL_UNIT_ASSIGNED_CONTEXT((#7836,#7838,#7839))
REPRESENTATION_CONTEXT('','3D')
);
#7826=(
GEOMETRIC_REPRESENTATION_CONTEXT(3)
GLOBAL_UNCERTAINTY_ASSIGNED_CONTEXT((#7800))
GLOBAL_UNIT_ASSIGNED_CONTEXT((#7836,#7838,#7839))
REPRESENTATION_CONTEXT('','3D')
);
#7827=(
GEOMETRIC_REPRESENTATION_CONTEXT(3)
GLOBAL_UNCERTAINTY_ASSIGNED_CONTEXT((#7801))
GLOBAL_UNIT_ASSIGNED_CONTEXT((#7836,#7838,#7839))
REPRESENTATION_CONTEXT('','3D')
);
#7828=(
GEOMETRIC_REPRESENTATION_CONTEXT(3)
GLOBAL_UNCERTAINTY_ASSIGNED_CONTEXT((#7802))
GLOBAL_UNIT_ASSIGNED_CONTEXT((#7836,#7838,#7839))
REPRESENTATION_CONTEXT('','3D')
);
#7829=(
GEOMETRIC_REPRESENTATION_CONTEXT(3)
GLOBAL_UNCERTAINTY_ASSIGNED_CONTEXT((#7803))
GLOBAL_UNIT_ASSIGNED_CONTEXT((#7836,#7838,#7839))
REPRESENTATION_CONTEXT('','3D')
);
#7830=(
GEOMETRIC_REPRESENTATION_CONTEXT(3)
GLOBAL_UNCERTAINTY_ASSIGNED_CONTEXT((#7804))
GLOBAL_UNIT_ASSIGNED_CONTEXT((#7836,#7838,#7839))
REPRESENTATION_CONTEXT('','3D')
);
#7831=(
GEOMETRIC_REPRESENTATION_CONTEXT(3)
GLOBAL_UNCERTAINTY_ASSIGNED_CONTEXT((#7805))
GLOBAL_UNIT_ASSIGNED_CONTEXT((#7836,#7838,#7839))
REPRESENTATION_CONTEXT('','3D')
);
#7832=(
GEOMETRIC_REPRESENTATION_CONTEXT(3)
GLOBAL_UNCERTAINTY_ASSIGNED_CONTEXT((#7806))
GLOBAL_UNIT_ASSIGNED_CONTEXT((#7836,#7838,#7839))
REPRESENTATION_CONTEXT('','3D')
);
#7833=(
GEOMETRIC_REPRESENTATION_CONTEXT(3)
GLOBAL_UNCERTAINTY_ASSIGNED_CONTEXT((#7807))
GLOBAL_UNIT_ASSIGNED_CONTEXT((#7836,#7838,#7839))
REPRESENTATION_CONTEXT('','3D')
);
#7834=(
GEOMETRIC_REPRESENTATION_CONTEXT(3)
GLOBAL_UNCERTAINTY_ASSIGNED_CONTEXT((#7808))
GLOBAL_UNIT_ASSIGNED_CONTEXT((#7836,#7838,#7839))
REPRESENTATION_CONTEXT('','3D')
);
#7835=(
GEOMETRIC_REPRESENTATION_CONTEXT(3)
GLOBAL_UNCERTAINTY_ASSIGNED_CONTEXT((#7809))
GLOBAL_UNIT_ASSIGNED_CONTEXT((#7836,#7838,#7839))
REPRESENTATION_CONTEXT('','3D')
);
#7836=(
LENGTH_UNIT()
NAMED_UNIT(*)
SI_UNIT(.CENTI.,.METRE.)
);
#7837=(
LENGTH_UNIT()
NAMED_UNIT(*)
SI_UNIT($,.METRE.)
);
#7838=(
NAMED_UNIT(*)
PLANE_ANGLE_UNIT()
SI_UNIT($,.RADIAN.)
);
#7839=(
NAMED_UNIT(*)
SI_UNIT($,.STERADIAN.)
SOLID_ANGLE_UNIT()
);
#7840=SHAPE_DEFINITION_REPRESENTATION(#7865,#7946);
#7841=SHAPE_DEFINITION_REPRESENTATION(#7866,#7947);
#7842=SHAPE_DEFINITION_REPRESENTATION(#7867,#7948);
#7843=SHAPE_DEFINITION_REPRESENTATION(#7868,#7949);
#7844=SHAPE_DEFINITION_REPRESENTATION(#7869,#7950);
#7845=SHAPE_DEFINITION_REPRESENTATION(#7870,#7951);
#7846=SHAPE_DEFINITION_REPRESENTATION(#7871,#7952);
#7847=SHAPE_DEFINITION_REPRESENTATION(#7872,#7953);
#7848=SHAPE_DEFINITION_REPRESENTATION(#7873,#7954);
#7849=SHAPE_DEFINITION_REPRESENTATION(#7874,#7955);
#7850=SHAPE_DEFINITION_REPRESENTATION(#7875,#7956);
#7851=SHAPE_DEFINITION_REPRESENTATION(#7876,#7957);
#7852=SHAPE_DEFINITION_REPRESENTATION(#7877,#7958);
#7853=SHAPE_DEFINITION_REPRESENTATION(#7878,#7959);
#7854=SHAPE_DEFINITION_REPRESENTATION(#7879,#7960);
#7855=SHAPE_DEFINITION_REPRESENTATION(#7880,#7961);
#7856=SHAPE_DEFINITION_REPRESENTATION(#7881,#7962);
#7857=SHAPE_DEFINITION_REPRESENTATION(#7882,#7963);
#7858=SHAPE_DEFINITION_REPRESENTATION(#7883,#7964);
#7859=SHAPE_DEFINITION_REPRESENTATION(#7884,#7965);
#7860=SHAPE_DEFINITION_REPRESENTATION(#7885,#7966);
#7861=SHAPE_DEFINITION_REPRESENTATION(#7888,#7967);
#7862=SHAPE_DEFINITION_REPRESENTATION(#7889,#7968);
#7863=SHAPE_DEFINITION_REPRESENTATION(#7917,#7969);
#7864=SHAPE_DEFINITION_REPRESENTATION(#7918,#7970);
#7865=PRODUCT_DEFINITION_SHAPE('',$,#7972);
#7866=PRODUCT_DEFINITION_SHAPE('',$,#7973);
#7867=PRODUCT_DEFINITION_SHAPE('',$,#7974);
#7868=PRODUCT_DEFINITION_SHAPE('',$,#7975);
#7869=PRODUCT_DEFINITION_SHAPE('',$,#7976);
#7870=PRODUCT_DEFINITION_SHAPE('',$,#7977);
#7871=PRODUCT_DEFINITION_SHAPE('',$,#7978);
#7872=PRODUCT_DEFINITION_SHAPE('',$,#7979);
#7873=PRODUCT_DEFINITION_SHAPE('',$,#7980);
#7874=PRODUCT_DEFINITION_SHAPE('',$,#7981);
#7875=PRODUCT_DEFINITION_SHAPE('',$,#7982);
#7876=PRODUCT_DEFINITION_SHAPE('',$,#7983);
#7877=PRODUCT_DEFINITION_SHAPE('',$,#7984);
#7878=PRODUCT_DEFINITION_SHAPE('',$,#7985);
#7879=PRODUCT_DEFINITION_SHAPE('',$,#7986);
#7880=PRODUCT_DEFINITION_SHAPE('',$,#7987);
#7881=PRODUCT_DEFINITION_SHAPE('',$,#7988);
#7882=PRODUCT_DEFINITION_SHAPE('',$,#7989);
#7883=PRODUCT_DEFINITION_SHAPE('',$,#7990);
#7884=PRODUCT_DEFINITION_SHAPE('',$,#7991);
#7885=PRODUCT_DEFINITION_SHAPE('',$,#7992);
#7886=PRODUCT_DEFINITION_SHAPE($,$,#179);
#7887=PRODUCT_DEFINITION_SHAPE($,$,#180);
#7888=PRODUCT_DEFINITION_SHAPE('',$,#7993);
#7889=PRODUCT_DEFINITION_SHAPE('',$,#7994);
#7890=PRODUCT_DEFINITION_SHAPE($,$,#181);
#7891=PRODUCT_DEFINITION_SHAPE($,$,#182);
#7892=PRODUCT_DEFINITION_SHAPE($,$,#183);
#7893=PRODUCT_DEFINITION_SHAPE($,$,#184);
#7894=PRODUCT_DEFINITION_SHAPE($,$,#185);
#7895=PRODUCT_DEFINITION_SHAPE($,$,#186);
#7896=PRODUCT_DEFINITION_SHAPE($,$,#187);
#7897=PRODUCT_DEFINITION_SHAPE($,$,#188);
#7898=PRODUCT_DEFINITION_SHAPE($,$,#189);
#7899=PRODUCT_DEFINITION_SHAPE($,$,#190);
#7900=PRODUCT_DEFINITION_SHAPE($,$,#191);
#7901=PRODUCT_DEFINITION_SHAPE($,$,#192);
#7902=PRODUCT_DEFINITION_SHAPE($,$,#193);
#7903=PRODUCT_DEFINITION_SHAPE($,$,#194);
#7904=PRODUCT_DEFINITION_SHAPE($,$,#195);
#7905=PRODUCT_DEFINITION_SHAPE($,$,#196);
#7906=PRODUCT_DEFINITION_SHAPE($,$,#197);
#7907=PRODUCT_DEFINITION_SHAPE($,$,#198);
#7908=PRODUCT_DEFINITION_SHAPE($,$,#199);
#7909=PRODUCT_DEFINITION_SHAPE($,$,#200);
#7910=PRODUCT_DEFINITION_SHAPE($,$,#201);
#7911=PRODUCT_DEFINITION_SHAPE($,$,#202);
#7912=PRODUCT_DEFINITION_SHAPE($,$,#203);
#7913=PRODUCT_DEFINITION_SHAPE($,$,#204);
#7914=PRODUCT_DEFINITION_SHAPE($,$,#205);
#7915=PRODUCT_DEFINITION_SHAPE($,$,#206);
#7916=PRODUCT_DEFINITION_SHAPE($,$,#207);
#7917=PRODUCT_DEFINITION_SHAPE('',$,#7995);
#7918=PRODUCT_DEFINITION_SHAPE('',$,#7996);
#7919=PRODUCT_DEFINITION_SHAPE($,$,#208);
#7920=PRODUCT_DEFINITION_SHAPE($,$,#209);
#7921=PRODUCT_DEFINITION_SHAPE($,$,#210);
#7922=PRODUCT_DEFINITION_SHAPE($,$,#211);
#7923=PRODUCT_DEFINITION_SHAPE($,$,#212);
#7924=PRODUCT_DEFINITION_SHAPE($,$,#213);
#7925=PRODUCT_DEFINITION_SHAPE($,$,#214);
#7926=PRODUCT_DEFINITION_SHAPE($,$,#215);
#7927=PRODUCT_DEFINITION_SHAPE($,$,#216);
#7928=PRODUCT_DEFINITION_SHAPE($,$,#217);
#7929=PRODUCT_DEFINITION_SHAPE($,$,#218);
#7930=PRODUCT_DEFINITION_SHAPE($,$,#219);
#7931=PRODUCT_DEFINITION_SHAPE($,$,#220);
#7932=PRODUCT_DEFINITION_SHAPE($,$,#221);
#7933=PRODUCT_DEFINITION_SHAPE($,$,#222);
#7934=PRODUCT_DEFINITION_SHAPE($,$,#223);
#7935=PRODUCT_DEFINITION_SHAPE($,$,#224);
#7936=PRODUCT_DEFINITION_SHAPE($,$,#225);
#7937=PRODUCT_DEFINITION_SHAPE($,$,#226);
#7938=PRODUCT_DEFINITION_SHAPE($,$,#227);
#7939=PRODUCT_DEFINITION_SHAPE($,$,#228);
#7940=PRODUCT_DEFINITION_SHAPE($,$,#229);
#7941=PRODUCT_DEFINITION_SHAPE($,$,#230);
#7942=PRODUCT_DEFINITION_SHAPE($,$,#231);
#7943=PRODUCT_DEFINITION_SHAPE($,$,#232);
#7944=PRODUCT_DEFINITION_SHAPE($,$,#233);
#7945=PRODUCT_DEFINITION_SHAPE($,$,#234);
#7946=SHAPE_REPRESENTATION('',(#4649,#5174,#5175),#7810);
#7947=SHAPE_REPRESENTATION('',(#4650,#5087,#5088,#5089,#5090,#5091,#5092,
#5093,#5094,#5095,#5096,#5097,#5098,#5099,#5100,#5101,#5102,#5103,#5104,
#5105,#5106,#5107,#5108,#5109,#5110,#5111,#5112,#5113),#7811);
#7948=SHAPE_REPRESENTATION('',(#4651),#7812);
#7949=SHAPE_REPRESENTATION('',(#4694),#7813);
#7950=SHAPE_REPRESENTATION('',(#4715),#7814);
#7951=SHAPE_REPRESENTATION('',(#4722),#7815);
#7952=SHAPE_REPRESENTATION('',(#4743),#7816);
#7953=SHAPE_REPRESENTATION('',(#4750),#7817);
#7954=SHAPE_REPRESENTATION('',(#4760),#7818);
#7955=SHAPE_REPRESENTATION('',(#4798),#7819);
#7956=SHAPE_REPRESENTATION('',(#4822,#5149,#5150,#5151,#5152,#5153,#5154,
#5155,#5156,#5157,#5158,#5159,#5160,#5161,#5162,#5163,#5164,#5165,#5166,
#5167,#5168,#5169,#5170,#5171,#5172,#5173),#7820);
#7957=SHAPE_REPRESENTATION('',(#4823),#7821);
#7958=SHAPE_REPRESENTATION('',(#4884),#7822);
#7959=SHAPE_REPRESENTATION('',(#4893),#7823);
#7960=SHAPE_REPRESENTATION('',(#4902),#7824);
#7961=SHAPE_REPRESENTATION('',(#4927),#7825);
#7962=SHAPE_REPRESENTATION('',(#4952),#7826);
#7963=SHAPE_REPRESENTATION('',(#4974),#7827);
#7964=SHAPE_REPRESENTATION('',(#4983,#5033,#5034),#7828);
#7965=SHAPE_REPRESENTATION('',(#4984),#7829);
#7966=SHAPE_REPRESENTATION('',(#5016),#7830);
#7967=SHAPE_REPRESENTATION('',(#5035),#7831);
#7968=SHAPE_REPRESENTATION('',(#5061),#7832);
#7969=SHAPE_REPRESENTATION('',(#5114),#7833);
#7970=SHAPE_REPRESENTATION('',(#5123),#7834);
#7971=PRODUCT_DEFINITION_CONTEXT('part definition',#8048,'design');
#7972=PRODUCT_DEFINITION('PAT-090',
'PAT-090',#7997,#7971);
#7973=PRODUCT_DEFINITION('Fixed frame','Fixed frame',#7998,#7971);
#7974=PRODUCT_DEFINITION('Base plate','Base plate',#7999,#7971);
#7975=PRODUCT_DEFINITION('End stop','End stop',#8000,#7971);
#7976=PRODUCT_DEFINITION('Bonded stop pad','Bonded stop pad',#8001,#7971);
#7977=PRODUCT_DEFINITION('End stop (1)','End stop (1)',#8002,#7971);
#7978=PRODUCT_DEFINITION('Bonded stop pad (1)','Bonded stop pad (1)',#8003,
#7971);
#7979=PRODUCT_DEFINITION(
'Precision Shaft - 12 mm Diameter, 300 mm Long',
'Precision Shaft - 12 mm Diameter, 300 mm Long',#8004,#7971);
#7980=PRODUCT_DEFINITION('Shaft Support - 12 mm Bore',
'Shaft Support - 12 mm Bore',#8005,#7971);
#7981=PRODUCT_DEFINITION('M5x14 Cap Screw','M5x14 Cap Screw',#8006,#7971);
#7982=PRODUCT_DEFINITION('Moving table','Moving table',#8007,#7971);
#7983=PRODUCT_DEFINITION('Bushing housing','Bushing housing',#8008,#7971);
#7984=PRODUCT_DEFINITION('Bushing spacer','Bushing spacer',#8009,#7971);
#7985=PRODUCT_DEFINITION('Bushing spacer (1)','Bushing spacer (1)',#8010,
#7971);
#7986=PRODUCT_DEFINITION('End retainer','End retainer',#8011,#7971);
#7987=PRODUCT_DEFINITION('End retainer (1)','End retainer (1)',#8012,#7971);
#7988=PRODUCT_DEFINITION('Table','Table',#8013,#7971);
#7989=PRODUCT_DEFINITION('Grip','Grip',#8014,#7971);
#7990=PRODUCT_DEFINITION('Linear Ball Bushing - 12 x 21 x 30 mm',
'Linear Ball Bushing - 12 x 21 x 30 mm',#8015,#7971);
#7991=PRODUCT_DEFINITION('Steel sleeve','Steel sleeve',#8016,#7971);
#7992=PRODUCT_DEFINITION('Ball retainer (plastic)',
'Ball retainer (plastic)',#8017,#7971);
#7993=PRODUCT_DEFINITION('Cap Screw - M4x16','Cap Screw - M4x16',#8018,
#7971);
#7994=PRODUCT_DEFINITION('Cap Screw - M5x20','Cap Screw - M5x20',#8019,
#7971);
#7995=PRODUCT_DEFINITION('Flat Washer - M6','Flat Washer - M6',#8020,#7971);
#7996=PRODUCT_DEFINITION('Cap Screw - M6x25','Cap Screw - M6x25',#8021,
#7971);
#7997=PRODUCT_DEFINITION_FORMATION('',$,#8050);
#7998=PRODUCT_DEFINITION_FORMATION('',$,#8051);
#7999=PRODUCT_DEFINITION_FORMATION('',$,#8052);
#8000=PRODUCT_DEFINITION_FORMATION('',$,#8053);
#8001=PRODUCT_DEFINITION_FORMATION('',$,#8054);
#8002=PRODUCT_DEFINITION_FORMATION('',$,#8055);
#8003=PRODUCT_DEFINITION_FORMATION('',$,#8056);
#8004=PRODUCT_DEFINITION_FORMATION('',$,#8057);
#8005=PRODUCT_DEFINITION_FORMATION('',$,#8058);
#8006=PRODUCT_DEFINITION_FORMATION('',$,#8059);
#8007=PRODUCT_DEFINITION_FORMATION('',$,#8060);
#8008=PRODUCT_DEFINITION_FORMATION('',$,#8061);
#8009=PRODUCT_DEFINITION_FORMATION('',$,#8062);
#8010=PRODUCT_DEFINITION_FORMATION('',$,#8063);
#8011=PRODUCT_DEFINITION_FORMATION('',$,#8064);
#8012=PRODUCT_DEFINITION_FORMATION('',$,#8065);
#8013=PRODUCT_DEFINITION_FORMATION('',$,#8066);
#8014=PRODUCT_DEFINITION_FORMATION('',$,#8067);
#8015=PRODUCT_DEFINITION_FORMATION('',$,#8068);
#8016=PRODUCT_DEFINITION_FORMATION('',$,#8069);
#8017=PRODUCT_DEFINITION_FORMATION('',$,#8070);
#8018=PRODUCT_DEFINITION_FORMATION('',$,#8071);
#8019=PRODUCT_DEFINITION_FORMATION('',$,#8072);
#8020=PRODUCT_DEFINITION_FORMATION('',$,#8073);
#8021=PRODUCT_DEFINITION_FORMATION('',$,#8074);
#8022=PRODUCT_RELATED_PRODUCT_CATEGORY('PAT-090','PAT-090',(#8050));
#8023=PRODUCT_RELATED_PRODUCT_CATEGORY('Fixed frame','Fixed frame',(#8051));
#8024=PRODUCT_RELATED_PRODUCT_CATEGORY('Base plate','Base plate',(#8052));
#8025=PRODUCT_RELATED_PRODUCT_CATEGORY('End stop','End stop',(#8053));
#8026=PRODUCT_RELATED_PRODUCT_CATEGORY('Bonded stop pad',
'Bonded stop pad',(#8054));
#8027=PRODUCT_RELATED_PRODUCT_CATEGORY('End stop (1)','End stop (1)',(#8055));
#8028=PRODUCT_RELATED_PRODUCT_CATEGORY('Bonded stop pad (1)',
'Bonded stop pad (1)',(#8056));
#8029=PRODUCT_RELATED_PRODUCT_CATEGORY(
'Precision Shaft - 12 mm Diameter, 300 mm Long',
'Precision Shaft - 12 mm Diameter, 300 mm Long',(#8057));
#8030=PRODUCT_RELATED_PRODUCT_CATEGORY('Shaft Support - 12 mm Bore',
'Shaft Support - 12 mm Bore',(#8058));
#8031=PRODUCT_RELATED_PRODUCT_CATEGORY('M5x14 Cap Screw',
'M5x14 Cap Screw',(#8059));
#8032=PRODUCT_RELATED_PRODUCT_CATEGORY('Moving table','Moving table',(#8060));
#8033=PRODUCT_RELATED_PRODUCT_CATEGORY('Bushing housing',
'Bushing housing',(#8061));
#8034=PRODUCT_RELATED_PRODUCT_CATEGORY('Bushing spacer',
'Bushing spacer',(#8062));
#8035=PRODUCT_RELATED_PRODUCT_CATEGORY('Bushing spacer (1)',
'Bushing spacer (1)',(#8063));
#8036=PRODUCT_RELATED_PRODUCT_CATEGORY('End retainer','End retainer',(#8064));
#8037=PRODUCT_RELATED_PRODUCT_CATEGORY('End retainer (1)',
'End retainer (1)',(#8065));
#8038=PRODUCT_RELATED_PRODUCT_CATEGORY('Table','Table',(#8066));
#8039=PRODUCT_RELATED_PRODUCT_CATEGORY('Grip','Grip',(#8067));
#8040=PRODUCT_RELATED_PRODUCT_CATEGORY(
'Linear Ball Bushing - 12 x 21 x 30 mm',
'Linear Ball Bushing - 12 x 21 x 30 mm',(#8068));
#8041=PRODUCT_RELATED_PRODUCT_CATEGORY('Steel sleeve','Steel sleeve',(#8069));
#8042=PRODUCT_RELATED_PRODUCT_CATEGORY('Ball retainer (plastic)',
'Ball retainer (plastic)',(#8070));
#8043=PRODUCT_RELATED_PRODUCT_CATEGORY('Cap Screw - M4x16',
'Cap Screw - M4x16',(#8071));
#8044=PRODUCT_RELATED_PRODUCT_CATEGORY('Cap Screw - M5x20',
'Cap Screw - M5x20',(#8072));
#8045=PRODUCT_RELATED_PRODUCT_CATEGORY('Flat Washer - M6',
'Flat Washer - M6',(#8073));
#8046=PRODUCT_RELATED_PRODUCT_CATEGORY('Cap Screw - M6x25',
'Cap Screw - M6x25',(#8074));
#8047=APPLICATION_PROTOCOL_DEFINITION('international standard',
'automotive_design',2009,#8048);
#8048=APPLICATION_CONTEXT(
'Core Data for Automotive Mechanical Design Process');
#8049=PRODUCT_CONTEXT('part definition',#8048,'mechanical');
#8050=PRODUCT('PAT-090','PAT-090',
'PAT-090',(#8049));
#8051=PRODUCT('Fixed frame','Fixed frame','Fixed frame',(#8049));
#8052=PRODUCT('Base plate','Base plate','Base plate',(#8049));
#8053=PRODUCT('End stop','End stop','End stop',(#8049));
#8054=PRODUCT('Bonded stop pad','Bonded stop pad','Bonded stop pad',(#8049));
#8055=PRODUCT('End stop (1)','End stop (1)','End stop (1)',(#8049));
#8056=PRODUCT('Bonded stop pad (1)','Bonded stop pad (1)',
'Bonded stop pad (1)',(#8049));
#8057=PRODUCT('Precision Shaft - 12 mm Diameter, 300 mm Long',
'Precision Shaft - 12 mm Diameter, 300 mm Long',
'Precision Shaft - 12 mm Diameter, 300 mm Long',(#8049));
#8058=PRODUCT('Shaft Support - 12 mm Bore','Shaft Support - 12 mm Bore',
'Shaft Support - 12 mm Bore',(#8049));
#8059=PRODUCT('M5x14 Cap Screw','M5x14 Cap Screw','M5x14 Cap Screw',(#8049));
#8060=PRODUCT('Moving table','Moving table','Moving table',(#8049));
#8061=PRODUCT('Bushing housing','Bushing housing','Bushing housing',(#8049));
#8062=PRODUCT('Bushing spacer','Bushing spacer','Bushing spacer',(#8049));
#8063=PRODUCT('Bushing spacer (1)','Bushing spacer (1)','Bushing spacer (1)',
(#8049));
#8064=PRODUCT('End retainer','End retainer','End retainer',(#8049));
#8065=PRODUCT('End retainer (1)','End retainer (1)','End retainer (1)',(#8049));
#8066=PRODUCT('Table','Table','Table',(#8049));
#8067=PRODUCT('Grip','Grip','Grip',(#8049));
#8068=PRODUCT('Linear Ball Bushing - 12 x 21 x 30 mm',
'Linear Ball Bushing - 12 x 21 x 30 mm',
'Linear Ball Bushing - 12 x 21 x 30 mm',(#8049));
#8069=PRODUCT('Steel sleeve','Steel sleeve','Steel sleeve',(#8049));
#8070=PRODUCT('Ball retainer (plastic)','Ball retainer (plastic)',
'Ball retainer (plastic)',(#8049));
#8071=PRODUCT('Cap Screw - M4x16','Cap Screw - M4x16',
'Cap Screw - M4x16',(#8049));
#8072=PRODUCT('Cap Screw - M5x20','Cap Screw - M5x20',
'Cap Screw - M5x20',(#8049));
#8073=PRODUCT('Flat Washer - M6','Flat Washer - M6','Flat Washer - M6',
(#8049));
#8074=PRODUCT('Cap Screw - M6x25','Cap Screw - M6x25',
'Cap Screw - M6x25',(#8049));
#8075=PRESENTATION_STYLE_ASSIGNMENT((#8081));
#8076=PRESENTATION_STYLE_ASSIGNMENT((#8082));
#8077=PRESENTATION_STYLE_ASSIGNMENT((#8083));
#8078=PRESENTATION_STYLE_ASSIGNMENT((#8084));
#8079=PRESENTATION_STYLE_ASSIGNMENT((#8085));
#8080=PRESENTATION_STYLE_ASSIGNMENT((#8086));
#8081=SURFACE_STYLE_USAGE(.BOTH.,#8087);
#8082=SURFACE_STYLE_USAGE(.BOTH.,#8088);
#8083=SURFACE_STYLE_USAGE(.BOTH.,#8089);
#8084=SURFACE_STYLE_USAGE(.BOTH.,#8090);
#8085=SURFACE_STYLE_USAGE(.BOTH.,#8091);
#8086=SURFACE_STYLE_USAGE(.BOTH.,#8092);
#8087=SURFACE_SIDE_STYLE('',(#8093));
#8088=SURFACE_SIDE_STYLE('',(#8094));
#8089=SURFACE_SIDE_STYLE('',(#8095));
#8090=SURFACE_SIDE_STYLE('',(#8096));
#8091=SURFACE_SIDE_STYLE('',(#8097));
#8092=SURFACE_SIDE_STYLE('',(#8098));
#8093=SURFACE_STYLE_FILL_AREA(#8099);
#8094=SURFACE_STYLE_FILL_AREA(#8100);
#8095=SURFACE_STYLE_FILL_AREA(#8101);
#8096=SURFACE_STYLE_FILL_AREA(#8102);
#8097=SURFACE_STYLE_FILL_AREA(#8103);
#8098=SURFACE_STYLE_FILL_AREA(#8104);
#8099=FILL_AREA_STYLE('Steel - Satin',(#8105));
#8100=FILL_AREA_STYLE('CAD Library Painted - Deep blue',(#8106));
#8101=FILL_AREA_STYLE('CAD Library Painted - Engineering blue',(#8107));
#8102=FILL_AREA_STYLE('CAD Library Painted - Graphite',(#8108));
#8103=FILL_AREA_STYLE('CAD Library Painted - Steel gray',(#8109));
#8104=FILL_AREA_STYLE('CAD Library Painted - Light blue',(#8110));
#8105=FILL_AREA_STYLE_COLOUR('Steel - Satin',#8111);
#8106=FILL_AREA_STYLE_COLOUR('CAD Library Painted - Deep blue',#8112);
#8107=FILL_AREA_STYLE_COLOUR('CAD Library Painted - Engineering blue',#8113);
#8108=FILL_AREA_STYLE_COLOUR('CAD Library Painted - Graphite',#8114);
#8109=FILL_AREA_STYLE_COLOUR('CAD Library Painted - Steel gray',#8115);
#8110=FILL_AREA_STYLE_COLOUR('CAD Library Painted - Light blue',#8116);
#8111=COLOUR_RGB('Steel - Satin',0.627450980392157,0.627450980392157,0.627450980392157);
#8112=COLOUR_RGB('CAD Library Painted - Deep blue',0.0784313725490196,0.203921568627451,
0.349019607843137);
#8113=COLOUR_RGB('CAD Library Painted - Engineering blue',0.12156862745098,
0.356862745098039,0.6);
#8114=COLOUR_RGB('CAD Library Painted - Graphite',0.168627450980392,0.192156862745098,
0.231372549019608);
#8115=COLOUR_RGB('CAD Library Painted - Steel gray',0.592156862745098,0.631372549019608,
0.67843137254902);
#8116=COLOUR_RGB('CAD Library Painted - Light blue',0.286274509803922,0.552941176470588,
0.780392156862745);
#8117=COLOUR_RGB('Dark Blue',0.08,0.2,0.34);
#8118=FILL_AREA_STYLE_COLOUR('',#8117);
#8119=FILL_AREA_STYLE('',(#8118));
#8120=SURFACE_STYLE_FILL_AREA(#8119);
#8121=SURFACE_SIDE_STYLE('',(#8120));
#8122=SURFACE_STYLE_USAGE(.BOTH.,#8121);
#8123=PRESENTATION_STYLE_ASSIGNMENT((#8122));
#8124=COLOUR_RGB('Light Blue',0.38,0.62,0.78);
#8125=FILL_AREA_STYLE_COLOUR('',#8124);
#8126=FILL_AREA_STYLE('',(#8125));
#8127=SURFACE_STYLE_FILL_AREA(#8126);
#8128=SURFACE_SIDE_STYLE('',(#8127));
#8129=SURFACE_STYLE_USAGE(.BOTH.,#8128);
#8130=PRESENTATION_STYLE_ASSIGNMENT((#8129));
#8131=COLOUR_RGB('Sky Blue',0.24,0.69,0.87);
#8132=FILL_AREA_STYLE_COLOUR('',#8131);
#8133=FILL_AREA_STYLE('',(#8132));
#8134=SURFACE_STYLE_FILL_AREA(#8133);
#8135=SURFACE_SIDE_STYLE('',(#8134));
#8136=SURFACE_STYLE_USAGE(.BOTH.,#8135);
#8137=PRESENTATION_STYLE_ASSIGNMENT((#8136));
#8138=COLOUR_RGB('Grey',0.48,0.52,0.57);
#8139=FILL_AREA_STYLE_COLOUR('',#8138);
#8140=FILL_AREA_STYLE('',(#8139));
#8141=SURFACE_STYLE_FILL_AREA(#8140);
#8142=SURFACE_SIDE_STYLE('',(#8141));
#8143=SURFACE_STYLE_USAGE(.BOTH.,#8142);
#8144=PRESENTATION_STYLE_ASSIGNMENT((#8143));
#8145=COLOUR_RGB('Black',0.12,0.14,0.17);
#8146=FILL_AREA_STYLE_COLOUR('',#8145);
#8147=FILL_AREA_STYLE('',(#8146));
#8148=SURFACE_STYLE_FILL_AREA(#8147);
#8149=SURFACE_SIDE_STYLE('',(#8148));
#8150=SURFACE_STYLE_USAGE(.BOTH.,#8149);
#8151=PRESENTATION_STYLE_ASSIGNMENT((#8150));
#8152=COLOUR_RGB('Off White',0.89,0.88,0.83);
#8153=FILL_AREA_STYLE_COLOUR('',#8152);
#8154=FILL_AREA_STYLE('',(#8153));
#8155=SURFACE_STYLE_FILL_AREA(#8154);
#8156=SURFACE_SIDE_STYLE('',(#8155));
#8157=SURFACE_STYLE_USAGE(.BOTH.,#8156);
#8158=PRESENTATION_STYLE_ASSIGNMENT((#8157));
ENDSEC;
END-ISO-10303-21;
